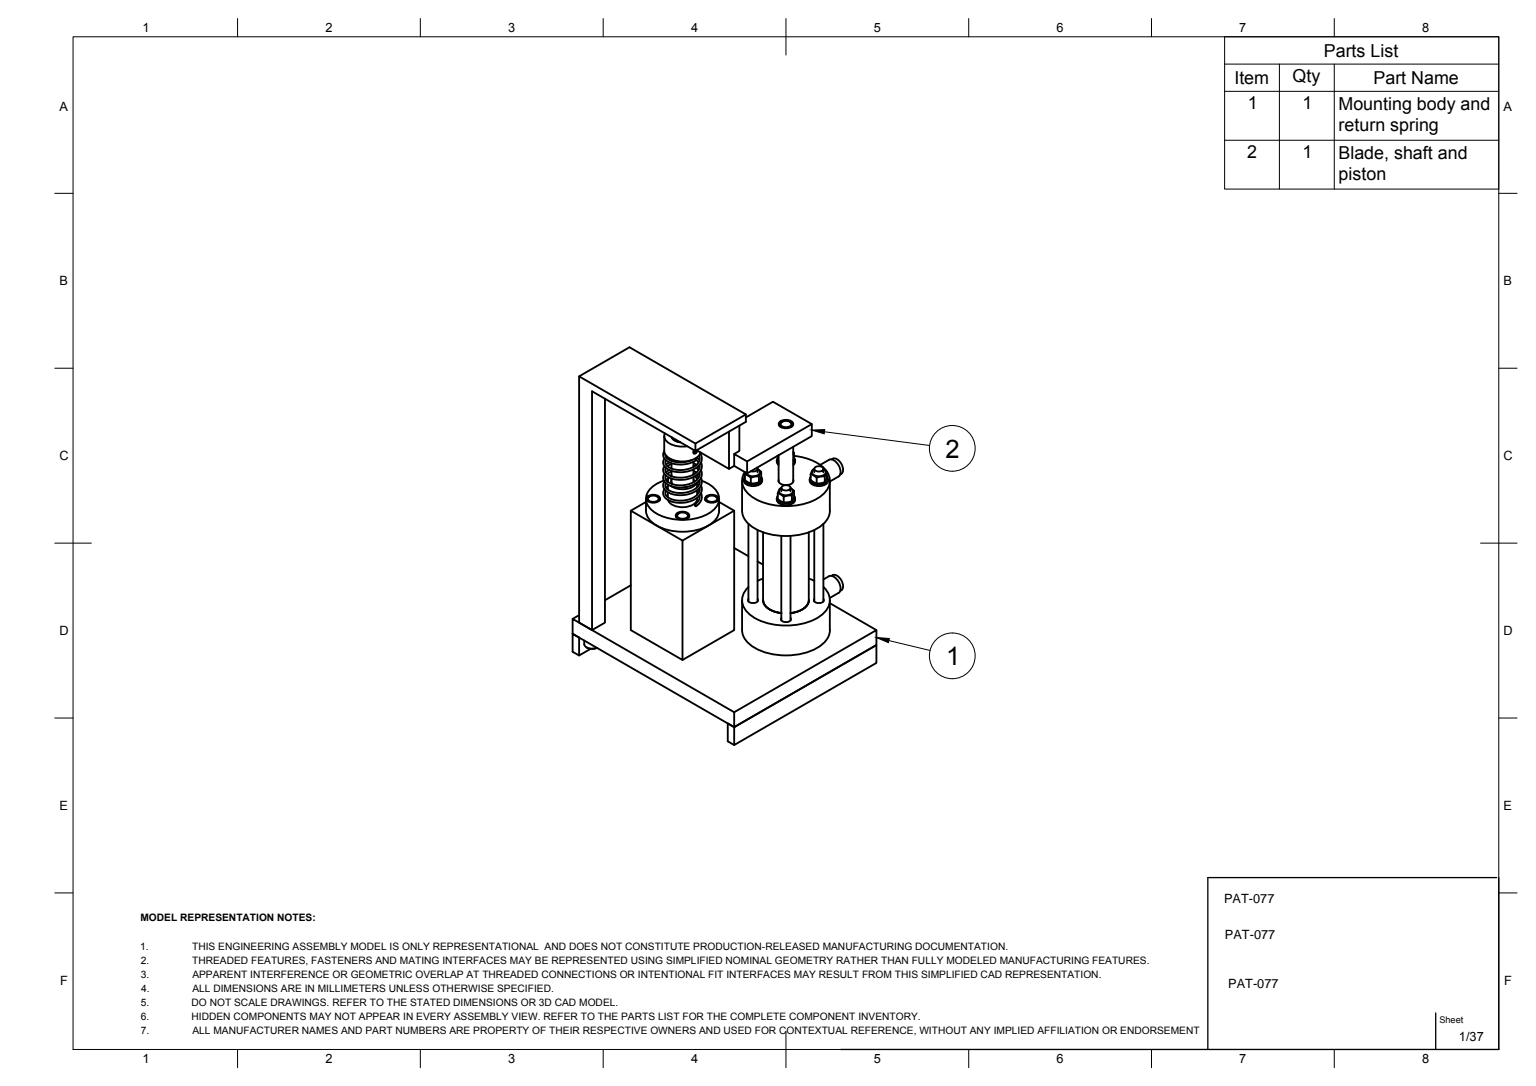
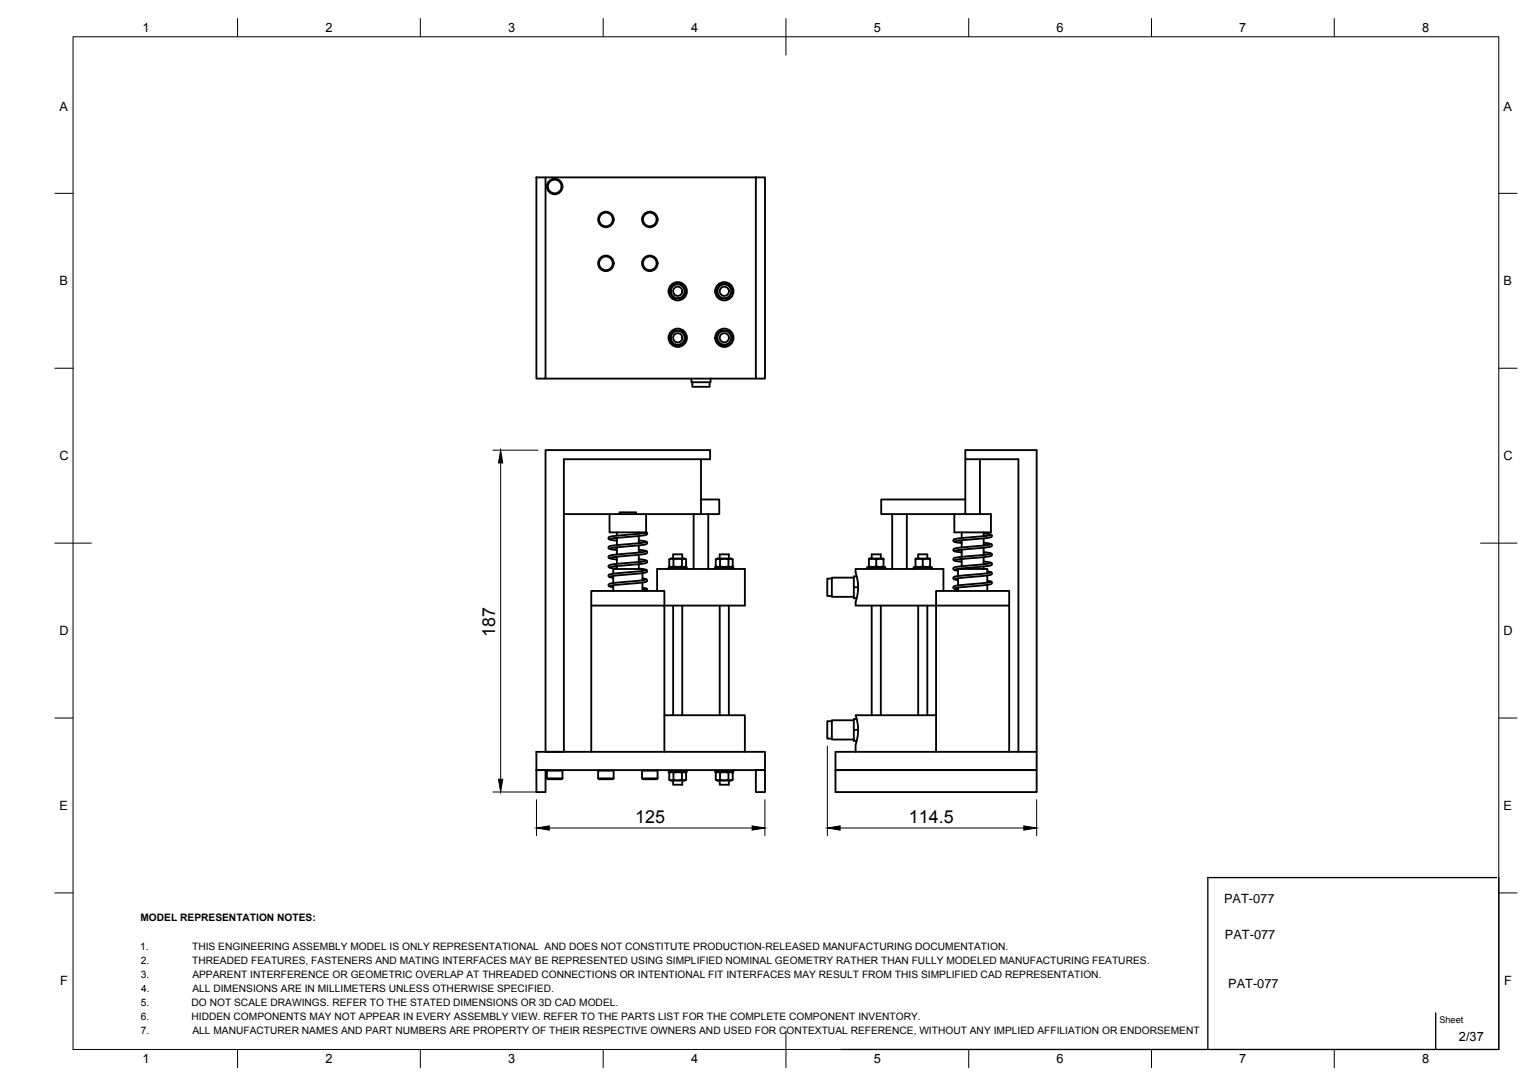
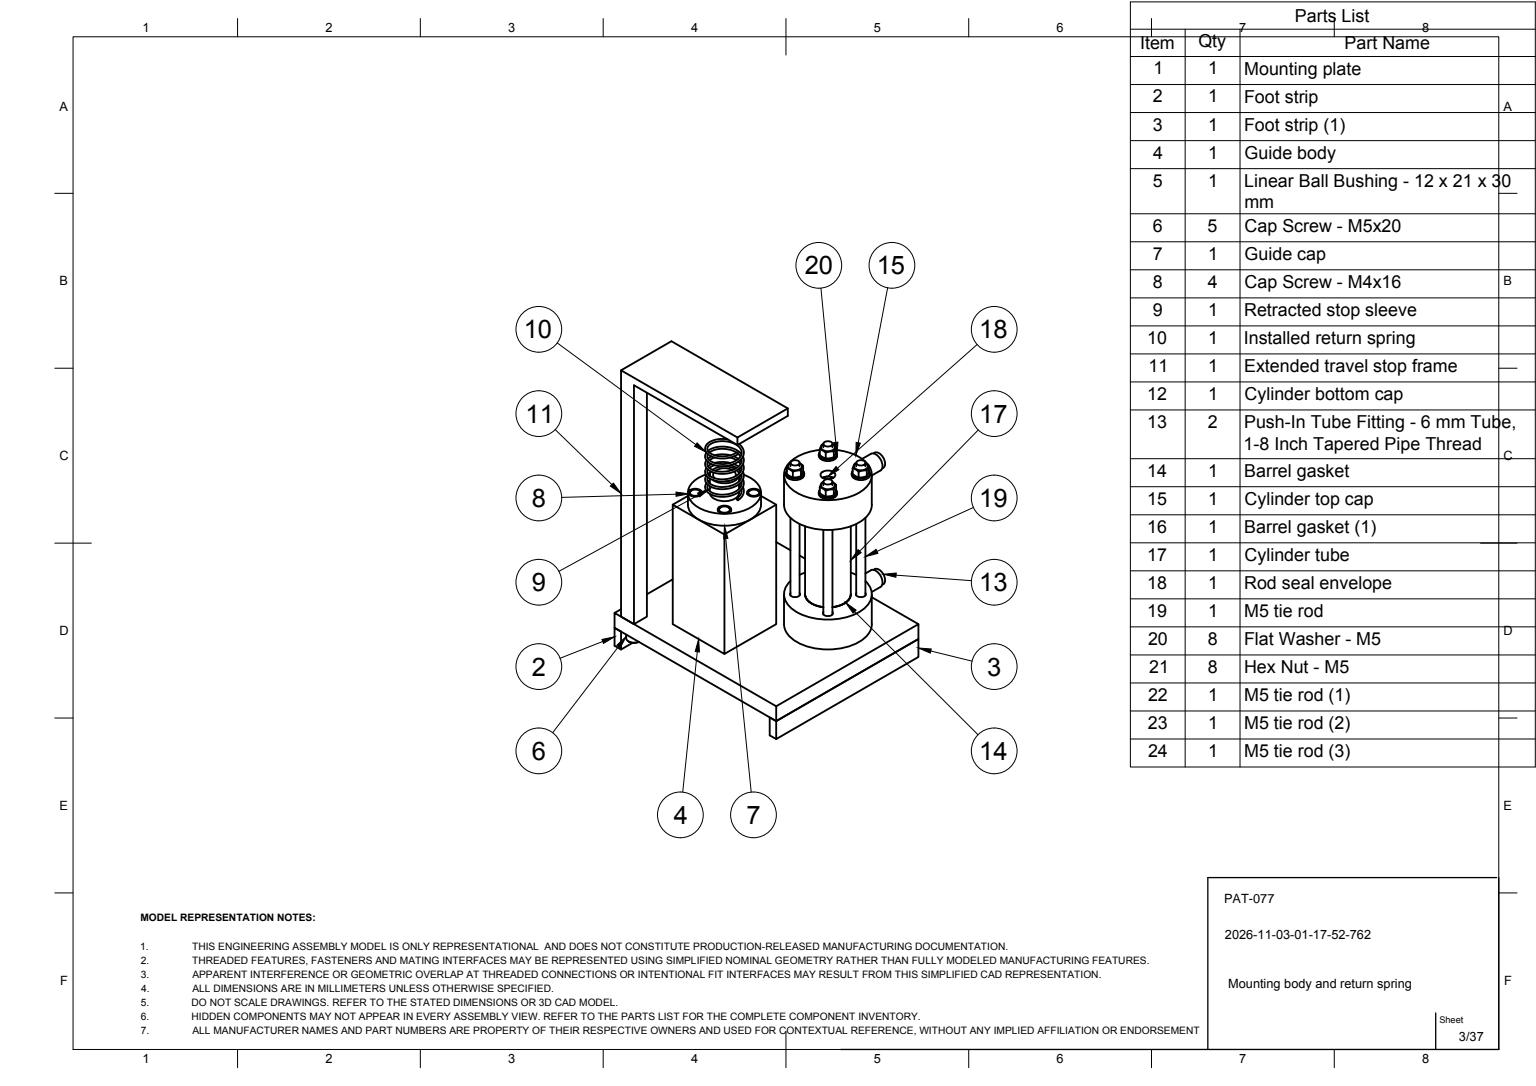
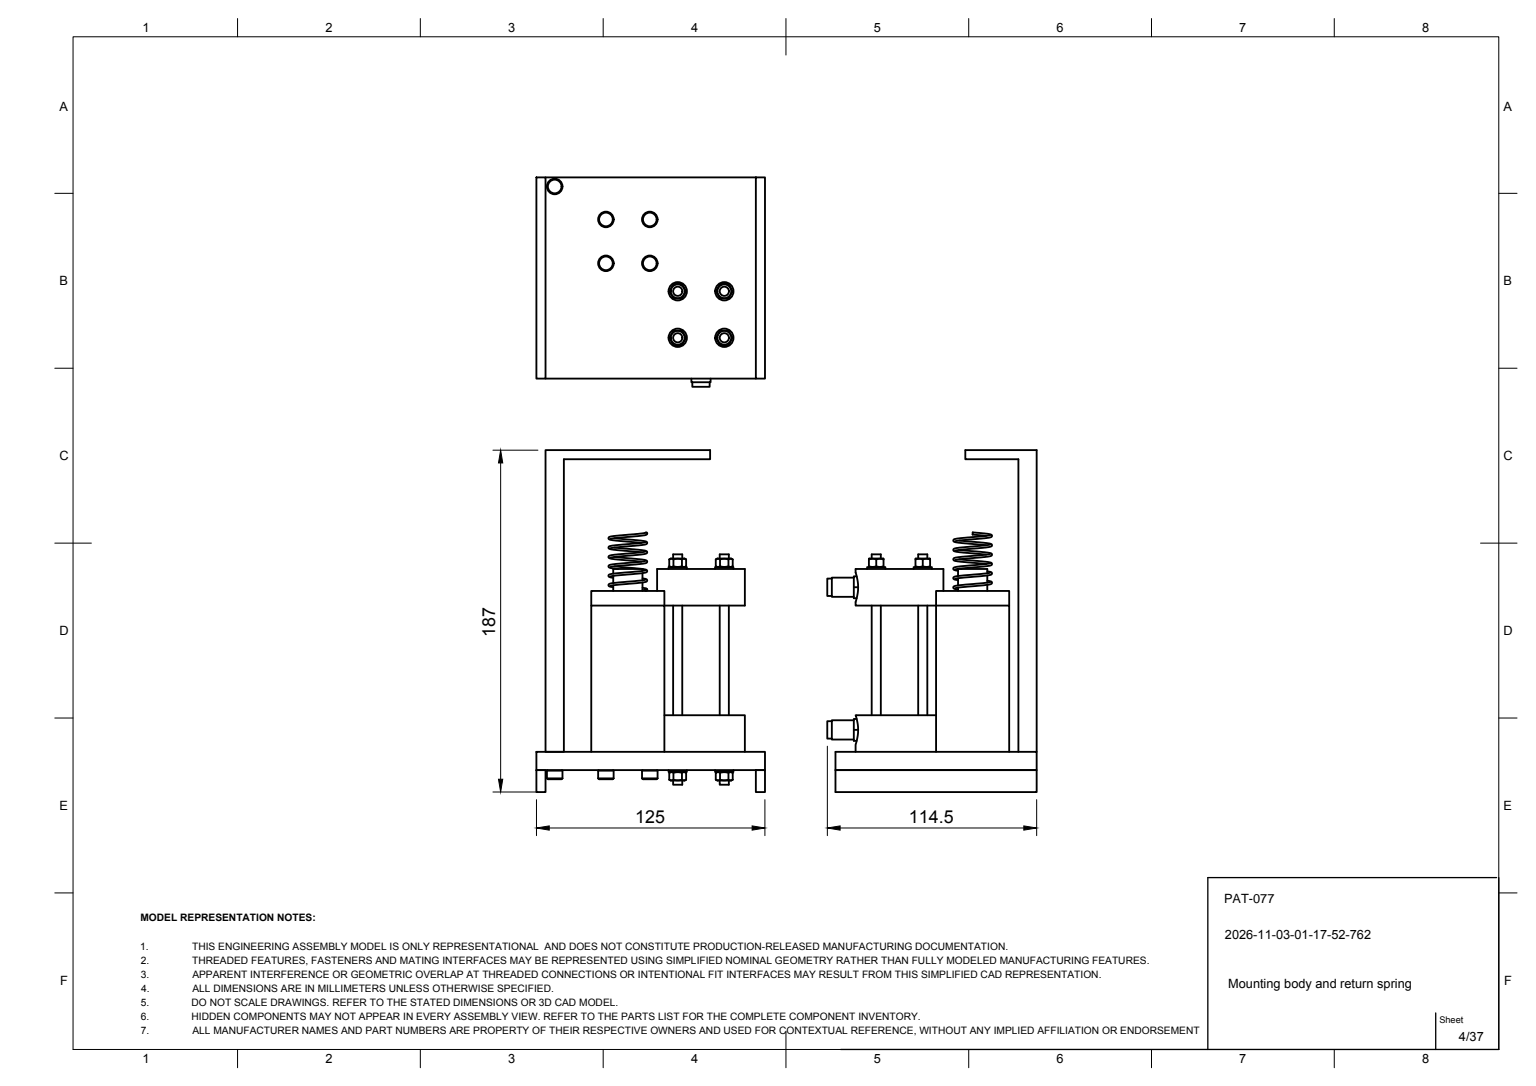
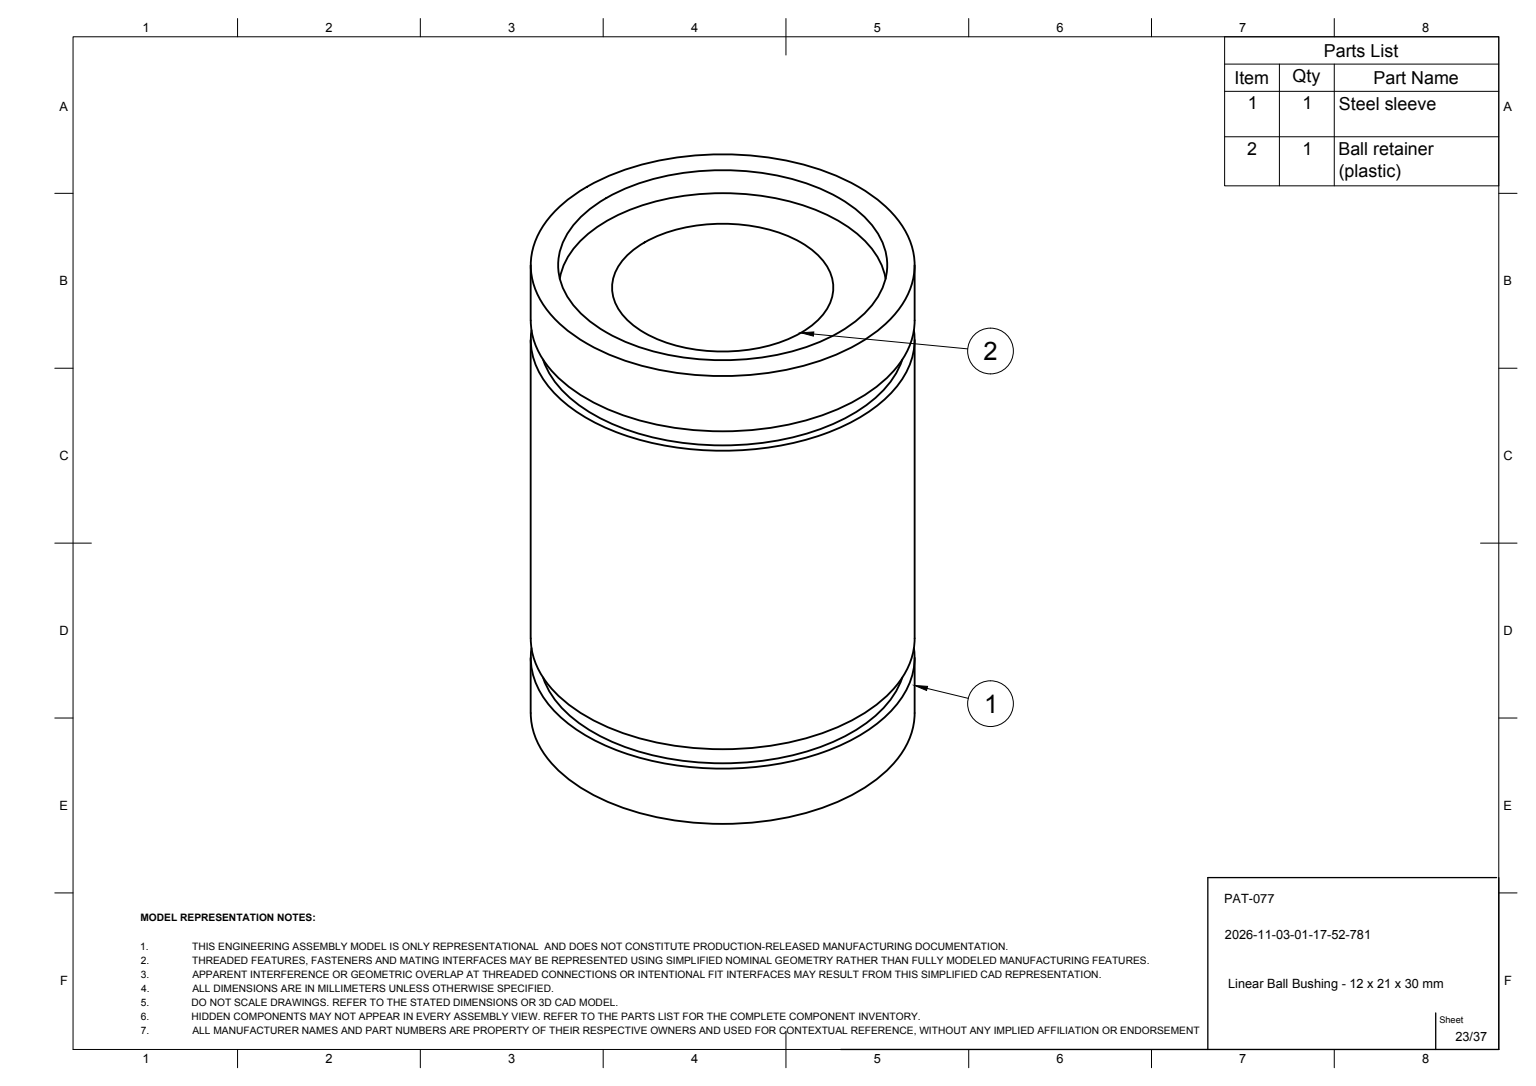
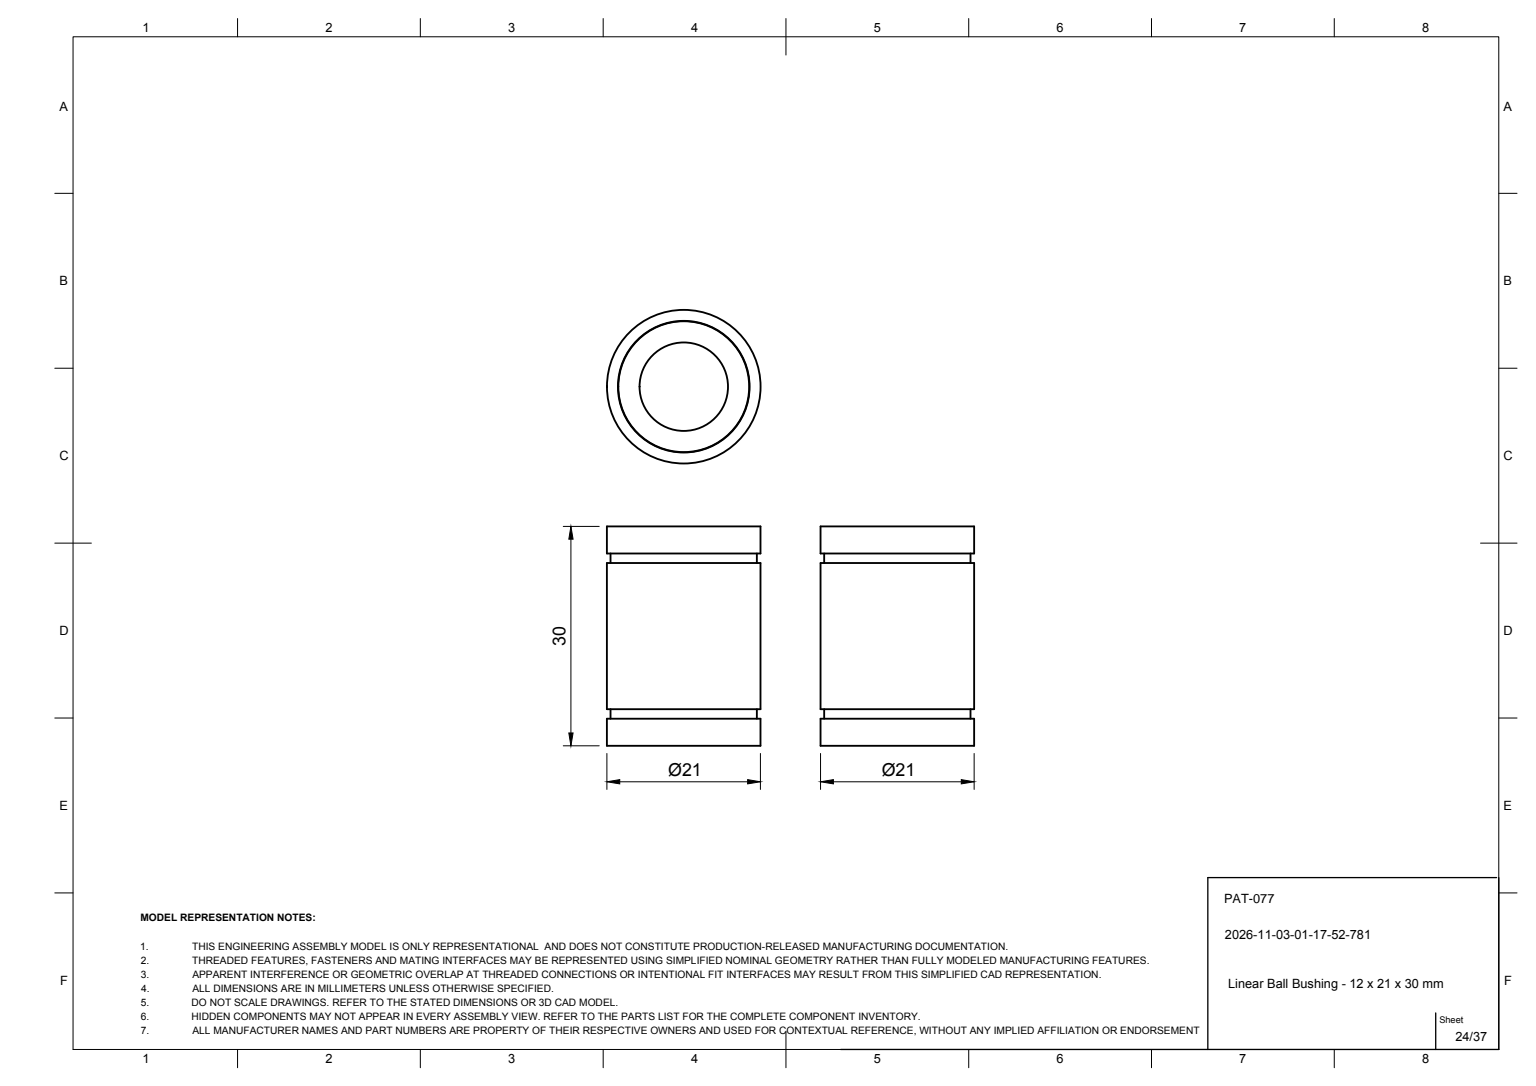
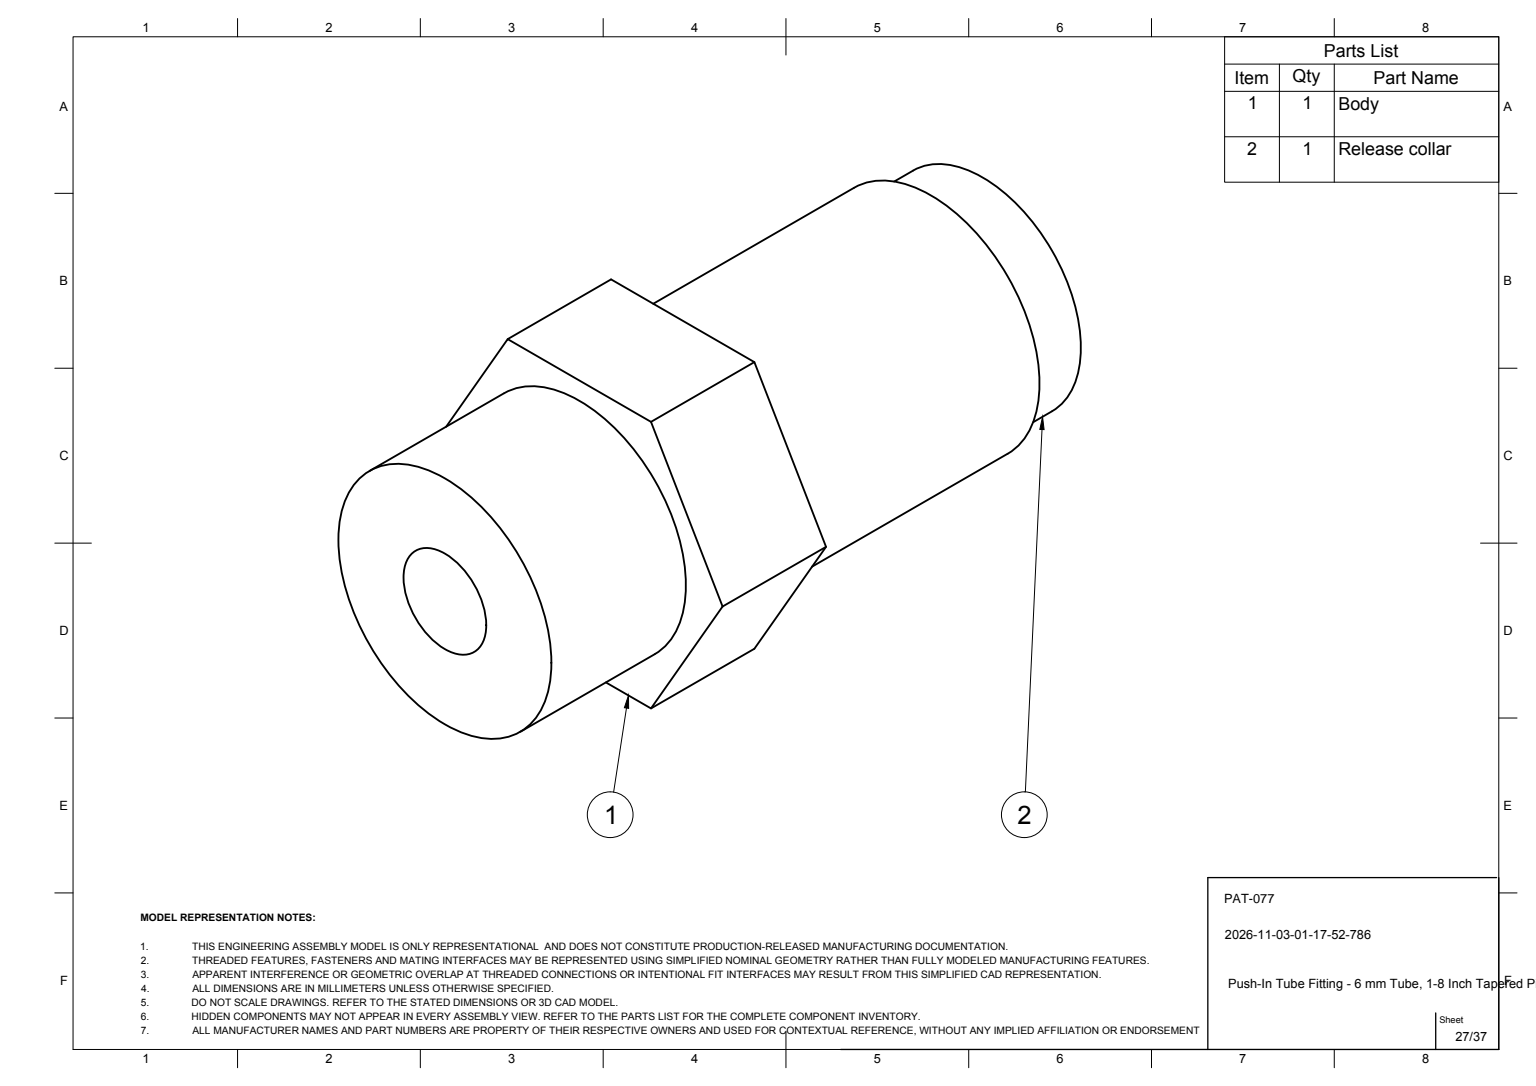
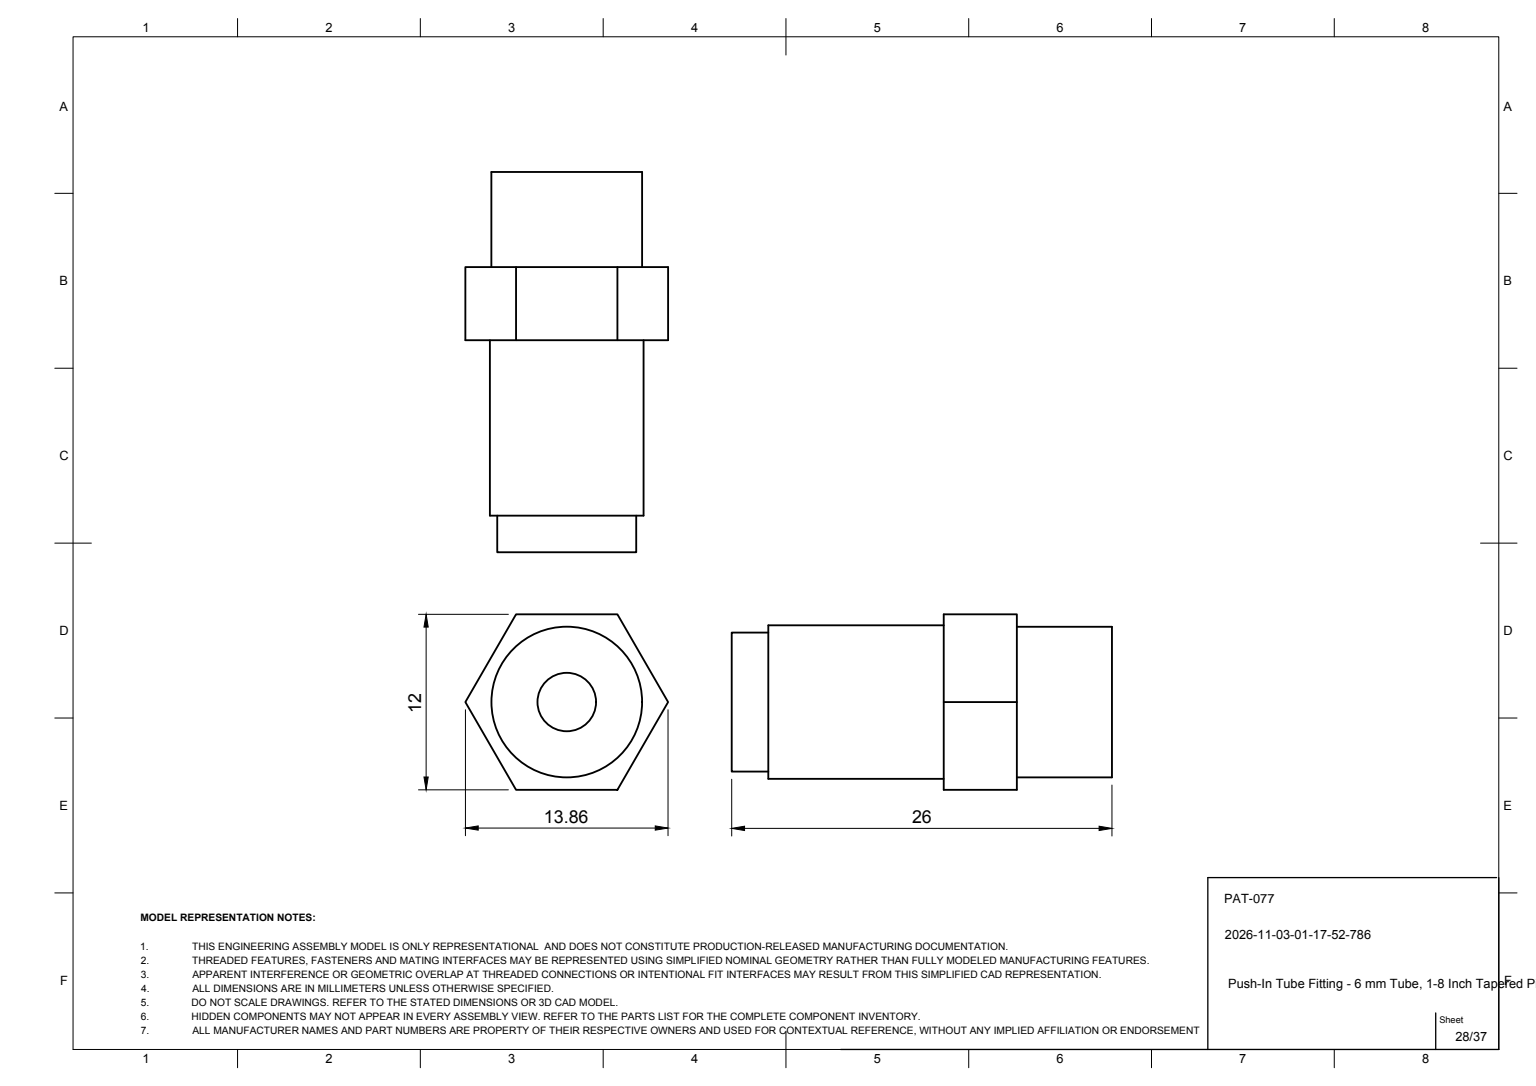
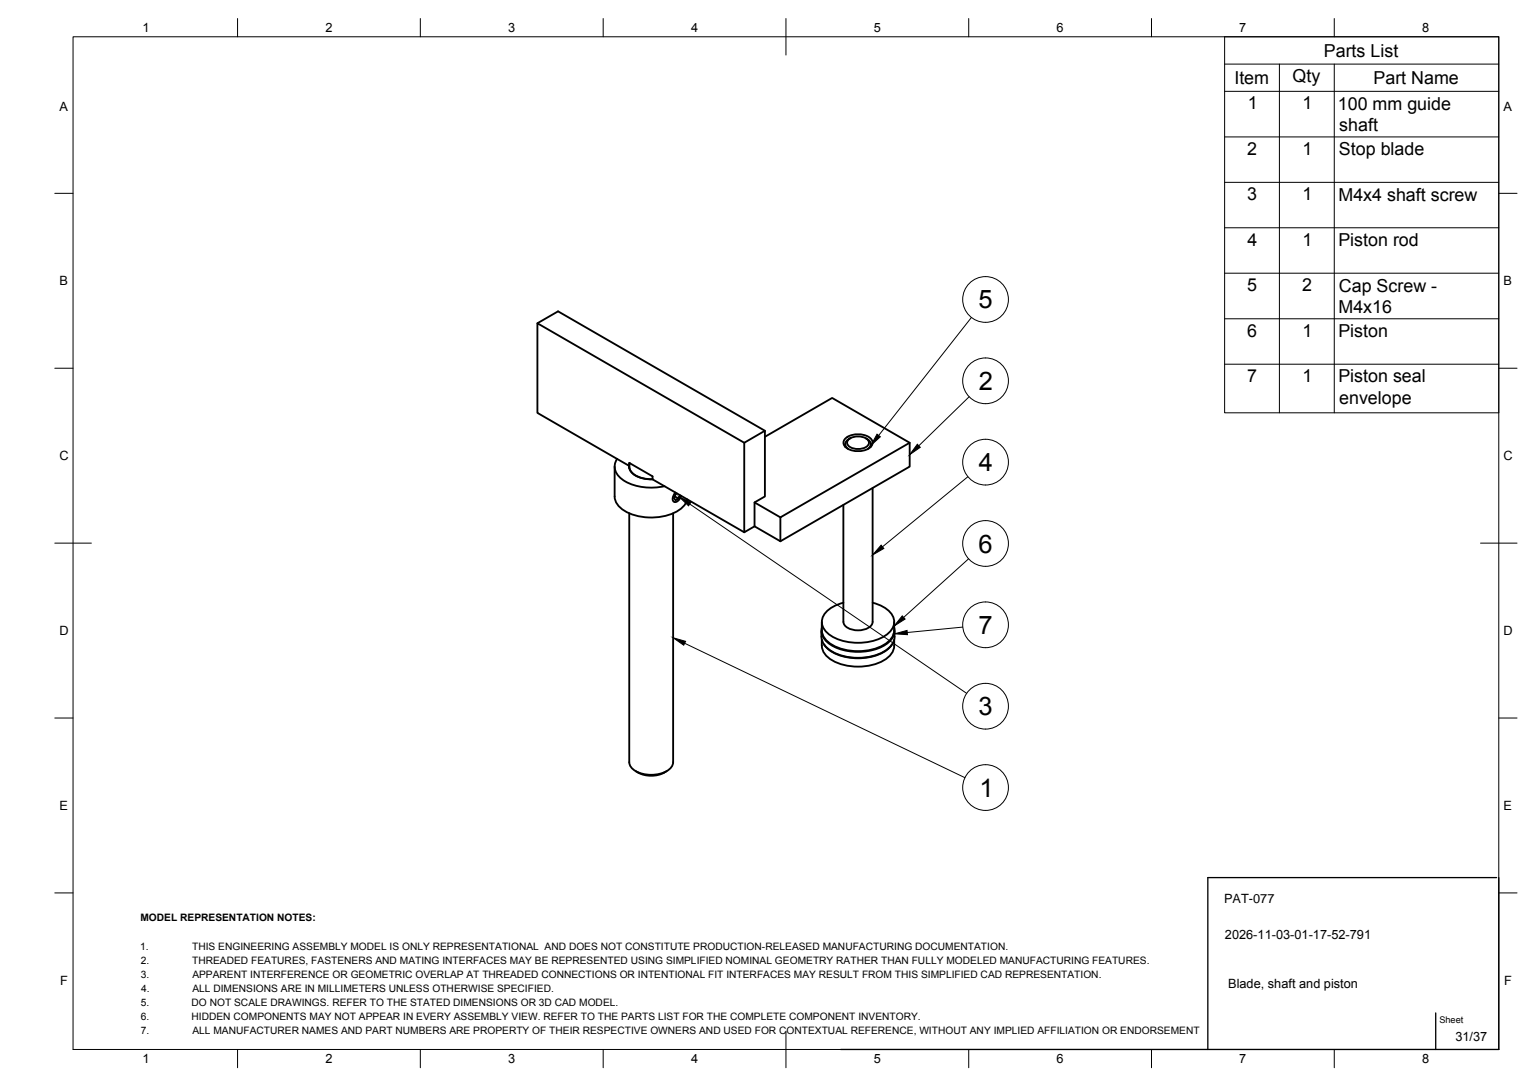
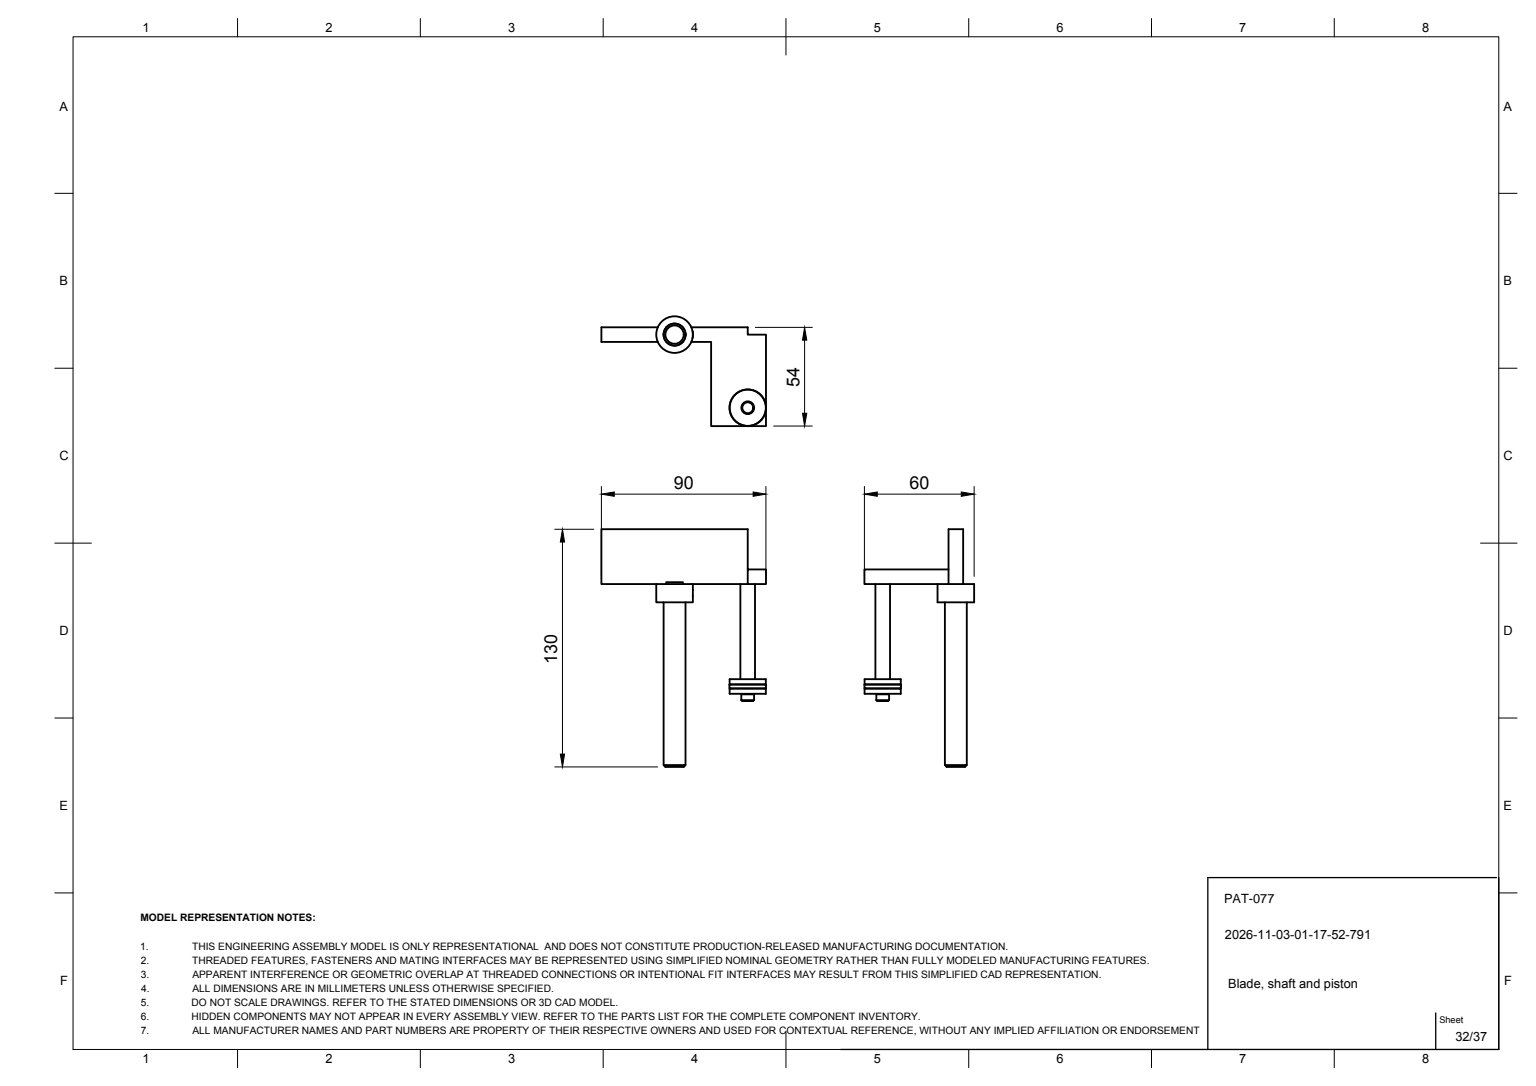
ISO-10303-21;
HEADER;
/* Generated by software containing ST-Developer
 * from STEP Tools, Inc. (www.steptools.com) 
 */

FILE_DESCRIPTION(
/* description */ ('Pallet stop with pneumatic fitting'),
/* implementation_level */ '2;1');

FILE_NAME(
/* name */ 'PAT-077',
/* time_stamp */ '2026-10-27T10:51:41-07:00',
/* author */ (''),
/* organization */ (''),
/* preprocessor_version */ 'ST-DEVELOPER v20.2',
/* originating_system */ 'Autodesk Translation Framework v15.17.0.0',
/* authorisation */ '');

FILE_SCHEMA (('AUTOMOTIVE_DESIGN { 1 0 10303 214 3 1 1 }'));
ENDSEC;

DATA;
#10=MECHANICAL_DESIGN_GEOMETRIC_PRESENTATION_REPRESENTATION('',(#357,#358,
#359,#360,#361,#362,#363,#364,#365,#366,#367,#368,#369,#370,#371,#372,#373,
#374,#375,#376,#377,#378,#379,#380,#381,#382,#383,#384,#385,#386,#387,#388),
#10265);
#11=(
BOUNDED_CURVE()
B_SPLINE_CURVE(2,(#9660,#9661,#9662),.UNSPECIFIED.,.F.,.F.)
B_SPLINE_CURVE_WITH_KNOTS((3,3),(0.140651836354967,0.670383167684795),
 .UNSPECIFIED.)
CURVE()
GEOMETRIC_REPRESENTATION_ITEM()
RATIONAL_B_SPLINE_CURVE((1.11602540378444,1.28867513459481,1.11602540378444))
REPRESENTATION_ITEM('')
);
#12=(
BOUNDED_CURVE()
B_SPLINE_CURVE(2,(#9664,#9665,#9666),.UNSPECIFIED.,.F.,.F.)
B_SPLINE_CURVE_WITH_KNOTS((3,3),(0.140651836354967,0.670383167684795),
 .UNSPECIFIED.)
CURVE()
GEOMETRIC_REPRESENTATION_ITEM()
RATIONAL_B_SPLINE_CURVE((1.11602540378444,1.28867513459481,1.11602540378444))
REPRESENTATION_ITEM('')
);
#13=(
BOUNDED_CURVE()
B_SPLINE_CURVE(2,(#9671,#9672,#9673),.UNSPECIFIED.,.F.,.F.)
B_SPLINE_CURVE_WITH_KNOTS((3,3),(0.140651836354967,0.670383167684795),
 .UNSPECIFIED.)
CURVE()
GEOMETRIC_REPRESENTATION_ITEM()
RATIONAL_B_SPLINE_CURVE((1.11602540378444,1.28867513459481,1.11602540378444))
REPRESENTATION_ITEM('')
);
#14=(
BOUNDED_CURVE()
B_SPLINE_CURVE(2,(#9675,#9676,#9677),.UNSPECIFIED.,.F.,.F.)
B_SPLINE_CURVE_WITH_KNOTS((3,3),(0.140651836354967,0.670383167684795),
 .UNSPECIFIED.)
CURVE()
GEOMETRIC_REPRESENTATION_ITEM()
RATIONAL_B_SPLINE_CURVE((1.11602540378444,1.28867513459481,1.11602540378444))
REPRESENTATION_ITEM('')
);
#15=(
BOUNDED_CURVE()
B_SPLINE_CURVE(2,(#9679,#9680,#9681),.UNSPECIFIED.,.F.,.F.)
B_SPLINE_CURVE_WITH_KNOTS((3,3),(0.140651836354967,0.670383167684795),
 .UNSPECIFIED.)
CURVE()
GEOMETRIC_REPRESENTATION_ITEM()
RATIONAL_B_SPLINE_CURVE((1.11602540378444,1.28867513459481,1.11602540378444))
REPRESENTATION_ITEM('')
);
#16=(
BOUNDED_CURVE()
B_SPLINE_CURVE(2,(#9682,#9683,#9684),.UNSPECIFIED.,.F.,.F.)
B_SPLINE_CURVE_WITH_KNOTS((3,3),(0.140651836354967,0.670383167684795),
 .UNSPECIFIED.)
CURVE()
GEOMETRIC_REPRESENTATION_ITEM()
RATIONAL_B_SPLINE_CURVE((1.11602540378444,1.28867513459481,1.11602540378444))
REPRESENTATION_ITEM('')
);
#17=(
BOUNDED_CURVE()
B_SPLINE_CURVE(2,(#9691,#9692,#9693),.UNSPECIFIED.,.F.,.F.)
B_SPLINE_CURVE_WITH_KNOTS((3,3),(0.140651836354967,0.670383167684795),
 .UNSPECIFIED.)
CURVE()
GEOMETRIC_REPRESENTATION_ITEM()
RATIONAL_B_SPLINE_CURVE((1.11602540378444,1.28867513459481,1.11602540378444))
REPRESENTATION_ITEM('')
);
#18=(
BOUNDED_CURVE()
B_SPLINE_CURVE(2,(#9695,#9696,#9697),.UNSPECIFIED.,.F.,.F.)
B_SPLINE_CURVE_WITH_KNOTS((3,3),(0.140651836354967,0.670383167684796),
 .UNSPECIFIED.)
CURVE()
GEOMETRIC_REPRESENTATION_ITEM()
RATIONAL_B_SPLINE_CURVE((1.11602540378444,1.28867513459481,1.11602540378444))
REPRESENTATION_ITEM('')
);
#19=(
BOUNDED_CURVE()
B_SPLINE_CURVE(2,(#9699,#9700,#9701),.UNSPECIFIED.,.F.,.F.)
B_SPLINE_CURVE_WITH_KNOTS((3,3),(0.140651836354967,0.670383167684795),
 .UNSPECIFIED.)
CURVE()
GEOMETRIC_REPRESENTATION_ITEM()
RATIONAL_B_SPLINE_CURVE((1.11602540378444,1.28867513459481,1.11602540378444))
REPRESENTATION_ITEM('')
);
#20=(
BOUNDED_CURVE()
B_SPLINE_CURVE(2,(#9703,#9704,#9705),.UNSPECIFIED.,.F.,.F.)
B_SPLINE_CURVE_WITH_KNOTS((3,3),(0.140651836354967,0.670383167684795),
 .UNSPECIFIED.)
CURVE()
GEOMETRIC_REPRESENTATION_ITEM()
RATIONAL_B_SPLINE_CURVE((1.11602540378444,1.28867513459482,1.11602540378444))
REPRESENTATION_ITEM('')
);
#21=(
BOUNDED_CURVE()
B_SPLINE_CURVE(2,(#9707,#9708,#9709),.UNSPECIFIED.,.F.,.F.)
B_SPLINE_CURVE_WITH_KNOTS((3,3),(0.140651836354967,0.670383167684795),
 .UNSPECIFIED.)
CURVE()
GEOMETRIC_REPRESENTATION_ITEM()
RATIONAL_B_SPLINE_CURVE((1.11602540378444,1.28867513459481,1.11602540378444))
REPRESENTATION_ITEM('')
);
#22=(
BOUNDED_CURVE()
B_SPLINE_CURVE(2,(#9710,#9711,#9712),.UNSPECIFIED.,.F.,.F.)
B_SPLINE_CURVE_WITH_KNOTS((3,3),(0.140651836354967,0.670383167684795),
 .UNSPECIFIED.)
CURVE()
GEOMETRIC_REPRESENTATION_ITEM()
RATIONAL_B_SPLINE_CURVE((1.11602540378444,1.28867513459481,1.11602540378444))
REPRESENTATION_ITEM('')
);
#23=ORIENTED_CLOSED_SHELL('',*,#5066,.F.);
#24=ORIENTED_CLOSED_SHELL('',*,#5078,.F.);
#25=CONICAL_SURFACE('',#5806,0.4,0.785398163397448);
#26=CONICAL_SURFACE('',#5810,0.41,0.785398163397448);
#27=CONICAL_SURFACE('',#5814,0.26,0.463647609000806);
#28=CONICAL_SURFACE('',#5818,0.225,0.785398163397448);
#29=CONICAL_SURFACE('',#5874,0.275,0.785398163397449);
#30=CONICAL_SURFACE('',#5885,0.47094010767585,1.0471975511966);
#31=CONICAL_SURFACE('',#5887,0.47094010767585,1.0471975511966);
#32=CONICAL_SURFACE('',#5987,0.55,0.785398163397448);
#33=CONICAL_SURFACE('',#6004,0.185,0.785398163397449);
#34=CONICAL_SURFACE('',#6010,0.325,0.785398163397448);
#35=CONICAL_SURFACE('',#6014,0.335,0.785398163397448);
#36=CONICAL_SURFACE('',#6018,0.21,0.463647609000806);
#37=CONICAL_SURFACE('',#6022,0.18,0.785398163397448);
#38=BREP_WITH_VOIDS('Body1',#5065,(#23));
#39=BREP_WITH_VOIDS('Body1',#5077,(#24));
#40=ITEM_DEFINED_TRANSFORMATION($,$,#5752,#5801);
#41=ITEM_DEFINED_TRANSFORMATION($,$,#5784,#5802);
#42=ITEM_DEFINED_TRANSFORMATION($,$,#5830,#5871);
#43=ITEM_DEFINED_TRANSFORMATION($,$,#5858,#5872);
#44=ITEM_DEFINED_TRANSFORMATION($,$,#5434,#6033);
#45=ITEM_DEFINED_TRANSFORMATION($,$,#5468,#6034);
#46=ITEM_DEFINED_TRANSFORMATION($,$,#5475,#6035);
#47=ITEM_DEFINED_TRANSFORMATION($,$,#5482,#6036);
#48=ITEM_DEFINED_TRANSFORMATION($,$,#5528,#6037);
#49=ITEM_DEFINED_TRANSFORMATION($,$,#5569,#6038);
#50=ITEM_DEFINED_TRANSFORMATION($,$,#5578,#6039);
#51=ITEM_DEFINED_TRANSFORMATION($,$,#5583,#6040);
#52=ITEM_DEFINED_TRANSFORMATION($,$,#5597,#6041);
#53=ITEM_DEFINED_TRANSFORMATION($,$,#5638,#6042);
#54=ITEM_DEFINED_TRANSFORMATION($,$,#5647,#6043);
#55=ITEM_DEFINED_TRANSFORMATION($,$,#5700,#6044);
#56=ITEM_DEFINED_TRANSFORMATION($,$,#5709,#6045);
#57=ITEM_DEFINED_TRANSFORMATION($,$,#5718,#6046);
#58=ITEM_DEFINED_TRANSFORMATION($,$,#5727,#6047);
#59=ITEM_DEFINED_TRANSFORMATION($,$,#5733,#6048);
#60=ITEM_DEFINED_TRANSFORMATION($,$,#5739,#6049);
#61=ITEM_DEFINED_TRANSFORMATION($,$,#5745,#6050);
#62=ITEM_DEFINED_TRANSFORMATION($,$,#5751,#6051);
#63=ITEM_DEFINED_TRANSFORMATION($,$,#5803,#6052);
#64=ITEM_DEFINED_TRANSFORMATION($,$,#5803,#6053);
#65=ITEM_DEFINED_TRANSFORMATION($,$,#5803,#6054);
#66=ITEM_DEFINED_TRANSFORMATION($,$,#5803,#6055);
#67=ITEM_DEFINED_TRANSFORMATION($,$,#6007,#6056);
#68=ITEM_DEFINED_TRANSFORMATION($,$,#6007,#6057);
#69=ITEM_DEFINED_TRANSFORMATION($,$,#6007,#6058);
#70=ITEM_DEFINED_TRANSFORMATION($,$,#6007,#6059);
#71=ITEM_DEFINED_TRANSFORMATION($,$,#5803,#6060);
#72=ITEM_DEFINED_TRANSFORMATION($,$,#5829,#6061);
#73=ITEM_DEFINED_TRANSFORMATION($,$,#5829,#6062);
#74=ITEM_DEFINED_TRANSFORMATION($,$,#5873,#6063);
#75=ITEM_DEFINED_TRANSFORMATION($,$,#5884,#6064);
#76=ITEM_DEFINED_TRANSFORMATION($,$,#5873,#6065);
#77=ITEM_DEFINED_TRANSFORMATION($,$,#5884,#6066);
#78=ITEM_DEFINED_TRANSFORMATION($,$,#5873,#6067);
#79=ITEM_DEFINED_TRANSFORMATION($,$,#5884,#6068);
#80=ITEM_DEFINED_TRANSFORMATION($,$,#5873,#6069);
#81=ITEM_DEFINED_TRANSFORMATION($,$,#5884,#6070);
#82=ITEM_DEFINED_TRANSFORMATION($,$,#5873,#6071);
#83=ITEM_DEFINED_TRANSFORMATION($,$,#5884,#6072);
#84=ITEM_DEFINED_TRANSFORMATION($,$,#5873,#6073);
#85=ITEM_DEFINED_TRANSFORMATION($,$,#5884,#6074);
#86=ITEM_DEFINED_TRANSFORMATION($,$,#5873,#6075);
#87=ITEM_DEFINED_TRANSFORMATION($,$,#5884,#6076);
#88=ITEM_DEFINED_TRANSFORMATION($,$,#5873,#6077);
#89=ITEM_DEFINED_TRANSFORMATION($,$,#5884,#6078);
#90=ITEM_DEFINED_TRANSFORMATION($,$,#5901,#6079);
#91=ITEM_DEFINED_TRANSFORMATION($,$,#5944,#6080);
#92=ITEM_DEFINED_TRANSFORMATION($,$,#5958,#6081);
#93=ITEM_DEFINED_TRANSFORMATION($,$,#5975,#6082);
#94=ITEM_DEFINED_TRANSFORMATION($,$,#5984,#6083);
#95=ITEM_DEFINED_TRANSFORMATION($,$,#5992,#6084);
#96=ITEM_DEFINED_TRANSFORMATION($,$,#6007,#6085);
#97=ITEM_DEFINED_TRANSFORMATION($,$,#6007,#6086);
#98=ITEM_DEFINED_TRANSFORMATION($,$,#5433,#6087);
#99=ITEM_DEFINED_TRANSFORMATION($,$,#5900,#6088);
#100=(
REPRESENTATION_RELATIONSHIP($,$,#10425,#10424)
REPRESENTATION_RELATIONSHIP_WITH_TRANSFORMATION(#40)
SHAPE_REPRESENTATION_RELATIONSHIP()
);
#101=(
REPRESENTATION_RELATIONSHIP($,$,#10426,#10424)
REPRESENTATION_RELATIONSHIP_WITH_TRANSFORMATION(#41)
SHAPE_REPRESENTATION_RELATIONSHIP()
);
#102=(
REPRESENTATION_RELATIONSHIP($,$,#10429,#10428)
REPRESENTATION_RELATIONSHIP_WITH_TRANSFORMATION(#42)
SHAPE_REPRESENTATION_RELATIONSHIP()
);
#103=(
REPRESENTATION_RELATIONSHIP($,$,#10430,#10428)
REPRESENTATION_RELATIONSHIP_WITH_TRANSFORMATION(#43)
SHAPE_REPRESENTATION_RELATIONSHIP()
);
#104=(
REPRESENTATION_RELATIONSHIP($,$,#10406,#10405)
REPRESENTATION_RELATIONSHIP_WITH_TRANSFORMATION(#44)
SHAPE_REPRESENTATION_RELATIONSHIP()
);
#105=(
REPRESENTATION_RELATIONSHIP($,$,#10407,#10405)
REPRESENTATION_RELATIONSHIP_WITH_TRANSFORMATION(#45)
SHAPE_REPRESENTATION_RELATIONSHIP()
);
#106=(
REPRESENTATION_RELATIONSHIP($,$,#10408,#10405)
REPRESENTATION_RELATIONSHIP_WITH_TRANSFORMATION(#46)
SHAPE_REPRESENTATION_RELATIONSHIP()
);
#107=(
REPRESENTATION_RELATIONSHIP($,$,#10409,#10405)
REPRESENTATION_RELATIONSHIP_WITH_TRANSFORMATION(#47)
SHAPE_REPRESENTATION_RELATIONSHIP()
);
#108=(
REPRESENTATION_RELATIONSHIP($,$,#10410,#10405)
REPRESENTATION_RELATIONSHIP_WITH_TRANSFORMATION(#48)
SHAPE_REPRESENTATION_RELATIONSHIP()
);
#109=(
REPRESENTATION_RELATIONSHIP($,$,#10411,#10405)
REPRESENTATION_RELATIONSHIP_WITH_TRANSFORMATION(#49)
SHAPE_REPRESENTATION_RELATIONSHIP()
);
#110=(
REPRESENTATION_RELATIONSHIP($,$,#10412,#10405)
REPRESENTATION_RELATIONSHIP_WITH_TRANSFORMATION(#50)
SHAPE_REPRESENTATION_RELATIONSHIP()
);
#111=(
REPRESENTATION_RELATIONSHIP($,$,#10413,#10405)
REPRESENTATION_RELATIONSHIP_WITH_TRANSFORMATION(#51)
SHAPE_REPRESENTATION_RELATIONSHIP()
);
#112=(
REPRESENTATION_RELATIONSHIP($,$,#10414,#10405)
REPRESENTATION_RELATIONSHIP_WITH_TRANSFORMATION(#52)
SHAPE_REPRESENTATION_RELATIONSHIP()
);
#113=(
REPRESENTATION_RELATIONSHIP($,$,#10415,#10405)
REPRESENTATION_RELATIONSHIP_WITH_TRANSFORMATION(#53)
SHAPE_REPRESENTATION_RELATIONSHIP()
);
#114=(
REPRESENTATION_RELATIONSHIP($,$,#10416,#10405)
REPRESENTATION_RELATIONSHIP_WITH_TRANSFORMATION(#54)
SHAPE_REPRESENTATION_RELATIONSHIP()
);
#115=(
REPRESENTATION_RELATIONSHIP($,$,#10417,#10405)
REPRESENTATION_RELATIONSHIP_WITH_TRANSFORMATION(#55)
SHAPE_REPRESENTATION_RELATIONSHIP()
);
#116=(
REPRESENTATION_RELATIONSHIP($,$,#10418,#10405)
REPRESENTATION_RELATIONSHIP_WITH_TRANSFORMATION(#56)
SHAPE_REPRESENTATION_RELATIONSHIP()
);
#117=(
REPRESENTATION_RELATIONSHIP($,$,#10419,#10405)
REPRESENTATION_RELATIONSHIP_WITH_TRANSFORMATION(#57)
SHAPE_REPRESENTATION_RELATIONSHIP()
);
#118=(
REPRESENTATION_RELATIONSHIP($,$,#10420,#10405)
REPRESENTATION_RELATIONSHIP_WITH_TRANSFORMATION(#58)
SHAPE_REPRESENTATION_RELATIONSHIP()
);
#119=(
REPRESENTATION_RELATIONSHIP($,$,#10421,#10405)
REPRESENTATION_RELATIONSHIP_WITH_TRANSFORMATION(#59)
SHAPE_REPRESENTATION_RELATIONSHIP()
);
#120=(
REPRESENTATION_RELATIONSHIP($,$,#10422,#10405)
REPRESENTATION_RELATIONSHIP_WITH_TRANSFORMATION(#60)
SHAPE_REPRESENTATION_RELATIONSHIP()
);
#121=(
REPRESENTATION_RELATIONSHIP($,$,#10423,#10405)
REPRESENTATION_RELATIONSHIP_WITH_TRANSFORMATION(#61)
SHAPE_REPRESENTATION_RELATIONSHIP()
);
#122=(
REPRESENTATION_RELATIONSHIP($,$,#10424,#10405)
REPRESENTATION_RELATIONSHIP_WITH_TRANSFORMATION(#62)
SHAPE_REPRESENTATION_RELATIONSHIP()
);
#123=(
REPRESENTATION_RELATIONSHIP($,$,#10427,#10405)
REPRESENTATION_RELATIONSHIP_WITH_TRANSFORMATION(#63)
SHAPE_REPRESENTATION_RELATIONSHIP()
);
#124=(
REPRESENTATION_RELATIONSHIP($,$,#10427,#10405)
REPRESENTATION_RELATIONSHIP_WITH_TRANSFORMATION(#64)
SHAPE_REPRESENTATION_RELATIONSHIP()
);
#125=(
REPRESENTATION_RELATIONSHIP($,$,#10427,#10405)
REPRESENTATION_RELATIONSHIP_WITH_TRANSFORMATION(#65)
SHAPE_REPRESENTATION_RELATIONSHIP()
);
#126=(
REPRESENTATION_RELATIONSHIP($,$,#10427,#10405)
REPRESENTATION_RELATIONSHIP_WITH_TRANSFORMATION(#66)
SHAPE_REPRESENTATION_RELATIONSHIP()
);
#127=(
REPRESENTATION_RELATIONSHIP($,$,#10440,#10405)
REPRESENTATION_RELATIONSHIP_WITH_TRANSFORMATION(#67)
SHAPE_REPRESENTATION_RELATIONSHIP()
);
#128=(
REPRESENTATION_RELATIONSHIP($,$,#10440,#10405)
REPRESENTATION_RELATIONSHIP_WITH_TRANSFORMATION(#68)
SHAPE_REPRESENTATION_RELATIONSHIP()
);
#129=(
REPRESENTATION_RELATIONSHIP($,$,#10440,#10405)
REPRESENTATION_RELATIONSHIP_WITH_TRANSFORMATION(#69)
SHAPE_REPRESENTATION_RELATIONSHIP()
);
#130=(
REPRESENTATION_RELATIONSHIP($,$,#10440,#10405)
REPRESENTATION_RELATIONSHIP_WITH_TRANSFORMATION(#70)
SHAPE_REPRESENTATION_RELATIONSHIP()
);
#131=(
REPRESENTATION_RELATIONSHIP($,$,#10427,#10405)
REPRESENTATION_RELATIONSHIP_WITH_TRANSFORMATION(#71)
SHAPE_REPRESENTATION_RELATIONSHIP()
);
#132=(
REPRESENTATION_RELATIONSHIP($,$,#10428,#10405)
REPRESENTATION_RELATIONSHIP_WITH_TRANSFORMATION(#72)
SHAPE_REPRESENTATION_RELATIONSHIP()
);
#133=(
REPRESENTATION_RELATIONSHIP($,$,#10428,#10405)
REPRESENTATION_RELATIONSHIP_WITH_TRANSFORMATION(#73)
SHAPE_REPRESENTATION_RELATIONSHIP()
);
#134=(
REPRESENTATION_RELATIONSHIP($,$,#10431,#10405)
REPRESENTATION_RELATIONSHIP_WITH_TRANSFORMATION(#74)
SHAPE_REPRESENTATION_RELATIONSHIP()
);
#135=(
REPRESENTATION_RELATIONSHIP($,$,#10432,#10405)
REPRESENTATION_RELATIONSHIP_WITH_TRANSFORMATION(#75)
SHAPE_REPRESENTATION_RELATIONSHIP()
);
#136=(
REPRESENTATION_RELATIONSHIP($,$,#10431,#10405)
REPRESENTATION_RELATIONSHIP_WITH_TRANSFORMATION(#76)
SHAPE_REPRESENTATION_RELATIONSHIP()
);
#137=(
REPRESENTATION_RELATIONSHIP($,$,#10432,#10405)
REPRESENTATION_RELATIONSHIP_WITH_TRANSFORMATION(#77)
SHAPE_REPRESENTATION_RELATIONSHIP()
);
#138=(
REPRESENTATION_RELATIONSHIP($,$,#10431,#10405)
REPRESENTATION_RELATIONSHIP_WITH_TRANSFORMATION(#78)
SHAPE_REPRESENTATION_RELATIONSHIP()
);
#139=(
REPRESENTATION_RELATIONSHIP($,$,#10432,#10405)
REPRESENTATION_RELATIONSHIP_WITH_TRANSFORMATION(#79)
SHAPE_REPRESENTATION_RELATIONSHIP()
);
#140=(
REPRESENTATION_RELATIONSHIP($,$,#10431,#10405)
REPRESENTATION_RELATIONSHIP_WITH_TRANSFORMATION(#80)
SHAPE_REPRESENTATION_RELATIONSHIP()
);
#141=(
REPRESENTATION_RELATIONSHIP($,$,#10432,#10405)
REPRESENTATION_RELATIONSHIP_WITH_TRANSFORMATION(#81)
SHAPE_REPRESENTATION_RELATIONSHIP()
);
#142=(
REPRESENTATION_RELATIONSHIP($,$,#10431,#10405)
REPRESENTATION_RELATIONSHIP_WITH_TRANSFORMATION(#82)
SHAPE_REPRESENTATION_RELATIONSHIP()
);
#143=(
REPRESENTATION_RELATIONSHIP($,$,#10432,#10405)
REPRESENTATION_RELATIONSHIP_WITH_TRANSFORMATION(#83)
SHAPE_REPRESENTATION_RELATIONSHIP()
);
#144=(
REPRESENTATION_RELATIONSHIP($,$,#10431,#10405)
REPRESENTATION_RELATIONSHIP_WITH_TRANSFORMATION(#84)
SHAPE_REPRESENTATION_RELATIONSHIP()
);
#145=(
REPRESENTATION_RELATIONSHIP($,$,#10432,#10405)
REPRESENTATION_RELATIONSHIP_WITH_TRANSFORMATION(#85)
SHAPE_REPRESENTATION_RELATIONSHIP()
);
#146=(
REPRESENTATION_RELATIONSHIP($,$,#10431,#10405)
REPRESENTATION_RELATIONSHIP_WITH_TRANSFORMATION(#86)
SHAPE_REPRESENTATION_RELATIONSHIP()
);
#147=(
REPRESENTATION_RELATIONSHIP($,$,#10432,#10405)
REPRESENTATION_RELATIONSHIP_WITH_TRANSFORMATION(#87)
SHAPE_REPRESENTATION_RELATIONSHIP()
);
#148=(
REPRESENTATION_RELATIONSHIP($,$,#10431,#10405)
REPRESENTATION_RELATIONSHIP_WITH_TRANSFORMATION(#88)
SHAPE_REPRESENTATION_RELATIONSHIP()
);
#149=(
REPRESENTATION_RELATIONSHIP($,$,#10432,#10405)
REPRESENTATION_RELATIONSHIP_WITH_TRANSFORMATION(#89)
SHAPE_REPRESENTATION_RELATIONSHIP()
);
#150=(
REPRESENTATION_RELATIONSHIP($,$,#10434,#10433)
REPRESENTATION_RELATIONSHIP_WITH_TRANSFORMATION(#90)
SHAPE_REPRESENTATION_RELATIONSHIP()
);
#151=(
REPRESENTATION_RELATIONSHIP($,$,#10435,#10433)
REPRESENTATION_RELATIONSHIP_WITH_TRANSFORMATION(#91)
SHAPE_REPRESENTATION_RELATIONSHIP()
);
#152=(
REPRESENTATION_RELATIONSHIP($,$,#10436,#10433)
REPRESENTATION_RELATIONSHIP_WITH_TRANSFORMATION(#92)
SHAPE_REPRESENTATION_RELATIONSHIP()
);
#153=(
REPRESENTATION_RELATIONSHIP($,$,#10437,#10433)
REPRESENTATION_RELATIONSHIP_WITH_TRANSFORMATION(#93)
SHAPE_REPRESENTATION_RELATIONSHIP()
);
#154=(
REPRESENTATION_RELATIONSHIP($,$,#10438,#10433)
REPRESENTATION_RELATIONSHIP_WITH_TRANSFORMATION(#94)
SHAPE_REPRESENTATION_RELATIONSHIP()
);
#155=(
REPRESENTATION_RELATIONSHIP($,$,#10439,#10433)
REPRESENTATION_RELATIONSHIP_WITH_TRANSFORMATION(#95)
SHAPE_REPRESENTATION_RELATIONSHIP()
);
#156=(
REPRESENTATION_RELATIONSHIP($,$,#10440,#10433)
REPRESENTATION_RELATIONSHIP_WITH_TRANSFORMATION(#96)
SHAPE_REPRESENTATION_RELATIONSHIP()
);
#157=(
REPRESENTATION_RELATIONSHIP($,$,#10440,#10433)
REPRESENTATION_RELATIONSHIP_WITH_TRANSFORMATION(#97)
SHAPE_REPRESENTATION_RELATIONSHIP()
);
#158=(
REPRESENTATION_RELATIONSHIP($,$,#10405,#10404)
REPRESENTATION_RELATIONSHIP_WITH_TRANSFORMATION(#98)
SHAPE_REPRESENTATION_RELATIONSHIP()
);
#159=(
REPRESENTATION_RELATIONSHIP($,$,#10433,#10404)
REPRESENTATION_RELATIONSHIP_WITH_TRANSFORMATION(#99)
SHAPE_REPRESENTATION_RELATIONSHIP()
);
#160=CONTEXT_DEPENDENT_SHAPE_REPRESENTATION(#100,#10330);
#161=CONTEXT_DEPENDENT_SHAPE_REPRESENTATION(#101,#10331);
#162=CONTEXT_DEPENDENT_SHAPE_REPRESENTATION(#102,#10336);
#163=CONTEXT_DEPENDENT_SHAPE_REPRESENTATION(#103,#10337);
#164=CONTEXT_DEPENDENT_SHAPE_REPRESENTATION(#104,#10348);
#165=CONTEXT_DEPENDENT_SHAPE_REPRESENTATION(#105,#10349);
#166=CONTEXT_DEPENDENT_SHAPE_REPRESENTATION(#106,#10350);
#167=CONTEXT_DEPENDENT_SHAPE_REPRESENTATION(#107,#10351);
#168=CONTEXT_DEPENDENT_SHAPE_REPRESENTATION(#108,#10352);
#169=CONTEXT_DEPENDENT_SHAPE_REPRESENTATION(#109,#10353);
#170=CONTEXT_DEPENDENT_SHAPE_REPRESENTATION(#110,#10354);
#171=CONTEXT_DEPENDENT_SHAPE_REPRESENTATION(#111,#10355);
#172=CONTEXT_DEPENDENT_SHAPE_REPRESENTATION(#112,#10356);
#173=CONTEXT_DEPENDENT_SHAPE_REPRESENTATION(#113,#10357);
#174=CONTEXT_DEPENDENT_SHAPE_REPRESENTATION(#114,#10358);
#175=CONTEXT_DEPENDENT_SHAPE_REPRESENTATION(#115,#10359);
#176=CONTEXT_DEPENDENT_SHAPE_REPRESENTATION(#116,#10360);
#177=CONTEXT_DEPENDENT_SHAPE_REPRESENTATION(#117,#10361);
#178=CONTEXT_DEPENDENT_SHAPE_REPRESENTATION(#118,#10362);
#179=CONTEXT_DEPENDENT_SHAPE_REPRESENTATION(#119,#10363);
#180=CONTEXT_DEPENDENT_SHAPE_REPRESENTATION(#120,#10364);
#181=CONTEXT_DEPENDENT_SHAPE_REPRESENTATION(#121,#10365);
#182=CONTEXT_DEPENDENT_SHAPE_REPRESENTATION(#122,#10366);
#183=CONTEXT_DEPENDENT_SHAPE_REPRESENTATION(#123,#10367);
#184=CONTEXT_DEPENDENT_SHAPE_REPRESENTATION(#124,#10368);
#185=CONTEXT_DEPENDENT_SHAPE_REPRESENTATION(#125,#10369);
#186=CONTEXT_DEPENDENT_SHAPE_REPRESENTATION(#126,#10370);
#187=CONTEXT_DEPENDENT_SHAPE_REPRESENTATION(#127,#10371);
#188=CONTEXT_DEPENDENT_SHAPE_REPRESENTATION(#128,#10372);
#189=CONTEXT_DEPENDENT_SHAPE_REPRESENTATION(#129,#10373);
#190=CONTEXT_DEPENDENT_SHAPE_REPRESENTATION(#130,#10374);
#191=CONTEXT_DEPENDENT_SHAPE_REPRESENTATION(#131,#10375);
#192=CONTEXT_DEPENDENT_SHAPE_REPRESENTATION(#132,#10376);
#193=CONTEXT_DEPENDENT_SHAPE_REPRESENTATION(#133,#10377);
#194=CONTEXT_DEPENDENT_SHAPE_REPRESENTATION(#134,#10378);
#195=CONTEXT_DEPENDENT_SHAPE_REPRESENTATION(#135,#10379);
#196=CONTEXT_DEPENDENT_SHAPE_REPRESENTATION(#136,#10380);
#197=CONTEXT_DEPENDENT_SHAPE_REPRESENTATION(#137,#10381);
#198=CONTEXT_DEPENDENT_SHAPE_REPRESENTATION(#138,#10382);
#199=CONTEXT_DEPENDENT_SHAPE_REPRESENTATION(#139,#10383);
#200=CONTEXT_DEPENDENT_SHAPE_REPRESENTATION(#140,#10384);
#201=CONTEXT_DEPENDENT_SHAPE_REPRESENTATION(#141,#10385);
#202=CONTEXT_DEPENDENT_SHAPE_REPRESENTATION(#142,#10386);
#203=CONTEXT_DEPENDENT_SHAPE_REPRESENTATION(#143,#10387);
#204=CONTEXT_DEPENDENT_SHAPE_REPRESENTATION(#144,#10388);
#205=CONTEXT_DEPENDENT_SHAPE_REPRESENTATION(#145,#10389);
#206=CONTEXT_DEPENDENT_SHAPE_REPRESENTATION(#146,#10390);
#207=CONTEXT_DEPENDENT_SHAPE_REPRESENTATION(#147,#10391);
#208=CONTEXT_DEPENDENT_SHAPE_REPRESENTATION(#148,#10392);
#209=CONTEXT_DEPENDENT_SHAPE_REPRESENTATION(#149,#10393);
#210=CONTEXT_DEPENDENT_SHAPE_REPRESENTATION(#150,#10394);
#211=CONTEXT_DEPENDENT_SHAPE_REPRESENTATION(#151,#10395);
#212=CONTEXT_DEPENDENT_SHAPE_REPRESENTATION(#152,#10396);
#213=CONTEXT_DEPENDENT_SHAPE_REPRESENTATION(#153,#10397);
#214=CONTEXT_DEPENDENT_SHAPE_REPRESENTATION(#154,#10398);
#215=CONTEXT_DEPENDENT_SHAPE_REPRESENTATION(#155,#10399);
#216=CONTEXT_DEPENDENT_SHAPE_REPRESENTATION(#156,#10400);
#217=CONTEXT_DEPENDENT_SHAPE_REPRESENTATION(#157,#10401);
#218=CONTEXT_DEPENDENT_SHAPE_REPRESENTATION(#158,#10402);
#219=CONTEXT_DEPENDENT_SHAPE_REPRESENTATION(#159,#10403);
#220=NEXT_ASSEMBLY_USAGE_OCCURRENCE('Steel sleeve:1','Steel sleeve:1',
'Steel sleeve:1',#10462,#10463,'Steel sleeve:1');
#221=NEXT_ASSEMBLY_USAGE_OCCURRENCE('Ball retainer (plastic):1',
'Ball retainer (plastic):1','Ball retainer (plastic):1',#10462,#10464,
'Ball retainer (plastic):1');
#222=NEXT_ASSEMBLY_USAGE_OCCURRENCE('Body:1','Body:1','Body:1',#10466,#10467,
'Body:1');
#223=NEXT_ASSEMBLY_USAGE_OCCURRENCE('Release collar:1',
'Release collar:1','Release collar:1',#10466,#10468,'Release collar:1');
#224=NEXT_ASSEMBLY_USAGE_OCCURRENCE('Mounting plate:1',
'Mounting plate:1','Mounting plate:1',#10443,#10444,'Mounting plate:1');
#225=NEXT_ASSEMBLY_USAGE_OCCURRENCE('Foot strip:1','Foot strip:1',
'Foot strip:1',#10443,#10445,'Foot strip:1');
#226=NEXT_ASSEMBLY_USAGE_OCCURRENCE('Foot strip (1):1',
'Foot strip (1):1','Foot strip (1):1',#10443,#10446,'Foot strip (1):1');
#227=NEXT_ASSEMBLY_USAGE_OCCURRENCE('Guide body:1','Guide body:1',
'Guide body:1',#10443,#10447,'Guide body:1');
#228=NEXT_ASSEMBLY_USAGE_OCCURRENCE('Guide cap:1','Guide cap:1',
'Guide cap:1',#10443,#10448,'Guide cap:1');
#229=NEXT_ASSEMBLY_USAGE_OCCURRENCE('Retracted stop sleeve:1',
'Retracted stop sleeve:1','Retracted stop sleeve:1',#10443,#10449,
'Retracted stop sleeve:1');
#230=NEXT_ASSEMBLY_USAGE_OCCURRENCE('Installed return spring:1',
'Installed return spring:1','Installed return spring:1',#10443,#10450,
'Installed return spring:1');
#231=NEXT_ASSEMBLY_USAGE_OCCURRENCE('Extended travel stop frame:1',
'Extended travel stop frame:1','Extended travel stop frame:1',#10443,#10451,
'Extended travel stop frame:1');
#232=NEXT_ASSEMBLY_USAGE_OCCURRENCE('Cylinder bottom cap:1',
'Cylinder bottom cap:1','Cylinder bottom cap:1',#10443,#10452,
'Cylinder bottom cap:1');
#233=NEXT_ASSEMBLY_USAGE_OCCURRENCE('Barrel gasket:1','Barrel gasket:1',
'Barrel gasket:1',#10443,#10453,'Barrel gasket:1');
#234=NEXT_ASSEMBLY_USAGE_OCCURRENCE('Cylinder top cap:1',
'Cylinder top cap:1','Cylinder top cap:1',#10443,#10454,
'Cylinder top cap:1');
#235=NEXT_ASSEMBLY_USAGE_OCCURRENCE('Barrel gasket (1):1',
'Barrel gasket (1):1','Barrel gasket (1):1',#10443,#10455,
'Barrel gasket (1):1');
#236=NEXT_ASSEMBLY_USAGE_OCCURRENCE('Cylinder tube:1','Cylinder tube:1',
'Cylinder tube:1',#10443,#10456,'Cylinder tube:1');
#237=NEXT_ASSEMBLY_USAGE_OCCURRENCE('Rod seal envelope:1',
'Rod seal envelope:1','Rod seal envelope:1',#10443,#10457,
'Rod seal envelope:1');
#238=NEXT_ASSEMBLY_USAGE_OCCURRENCE('M5 tie rod:1','M5 tie rod:1',
'M5 tie rod:1',#10443,#10458,'M5 tie rod:1');
#239=NEXT_ASSEMBLY_USAGE_OCCURRENCE('M5 tie rod (1):1',
'M5 tie rod (1):1','M5 tie rod (1):1',#10443,#10459,'M5 tie rod (1):1');
#240=NEXT_ASSEMBLY_USAGE_OCCURRENCE('M5 tie rod (2):1',
'M5 tie rod (2):1','M5 tie rod (2):1',#10443,#10460,'M5 tie rod (2):1');
#241=NEXT_ASSEMBLY_USAGE_OCCURRENCE('M5 tie rod (3):1',
'M5 tie rod (3):1','M5 tie rod (3):1',#10443,#10461,'M5 tie rod (3):1');
#242=NEXT_ASSEMBLY_USAGE_OCCURRENCE(
'Linear Ball Bushing - 12 x 21 x 30 mm:2',
'Linear Ball Bushing - 12 x 21 x 30 mm:2',
'Linear Ball Bushing - 12 x 21 x 30 mm:2',#10443,#10462,
'Linear Ball Bushing - 12 x 21 x 30 mm:2');
#243=NEXT_ASSEMBLY_USAGE_OCCURRENCE('Cap Screw - M5x20:2',
'Cap Screw - M5x20:2','Cap Screw - M5x20:2',#10443,#10465,
'Cap Screw - M5x20:2');
#244=NEXT_ASSEMBLY_USAGE_OCCURRENCE('Cap Screw - M5x20:3',
'Cap Screw - M5x20:3','Cap Screw - M5x20:3',#10443,#10465,
'Cap Screw - M5x20:3');
#245=NEXT_ASSEMBLY_USAGE_OCCURRENCE('Cap Screw - M5x20:4',
'Cap Screw - M5x20:4','Cap Screw - M5x20:4',#10443,#10465,
'Cap Screw - M5x20:4');
#246=NEXT_ASSEMBLY_USAGE_OCCURRENCE('Cap Screw - M5x20:5',
'Cap Screw - M5x20:5','Cap Screw - M5x20:5',#10443,#10465,
'Cap Screw - M5x20:5');
#247=NEXT_ASSEMBLY_USAGE_OCCURRENCE('Cap Screw - M4x16:2',
'Cap Screw - M4x16:2','Cap Screw - M4x16:2',#10443,#10478,
'Cap Screw - M4x16:2');
#248=NEXT_ASSEMBLY_USAGE_OCCURRENCE('Cap Screw - M4x16:3',
'Cap Screw - M4x16:3','Cap Screw - M4x16:3',#10443,#10478,
'Cap Screw - M4x16:3');
#249=NEXT_ASSEMBLY_USAGE_OCCURRENCE('Cap Screw - M4x16:4',
'Cap Screw - M4x16:4','Cap Screw - M4x16:4',#10443,#10478,
'Cap Screw - M4x16:4');
#250=NEXT_ASSEMBLY_USAGE_OCCURRENCE('Cap Screw - M4x16:5',
'Cap Screw - M4x16:5','Cap Screw - M4x16:5',#10443,#10478,
'Cap Screw - M4x16:5');
#251=NEXT_ASSEMBLY_USAGE_OCCURRENCE('Cap Screw - M5x20:6',
'Cap Screw - M5x20:6','Cap Screw - M5x20:6',#10443,#10465,
'Cap Screw - M5x20:6');
#252=NEXT_ASSEMBLY_USAGE_OCCURRENCE(
'Push-In Tube Fitting - 6 mm Tube, 1-8 Inch Tapered Pipe Thread:2',
'Push-In Tube Fitting - 6 mm Tube, 1-8 Inch Tapered Pipe Thread:2',
'Push-In Tube Fitting - 6 mm Tube, 1-8 Inch Tapered Pipe Thread:2',#10443,
#10466,
'Push-In Tube Fitting - 6 mm Tube, 1-8 Inch Tapered Pipe Thread:2');
#253=NEXT_ASSEMBLY_USAGE_OCCURRENCE(
'Push-In Tube Fitting - 6 mm Tube, 1-8 Inch Tapered Pipe Thread:3',
'Push-In Tube Fitting - 6 mm Tube, 1-8 Inch Tapered Pipe Thread:3',
'Push-In Tube Fitting - 6 mm Tube, 1-8 Inch Tapered Pipe Thread:3',#10443,
#10466,
'Push-In Tube Fitting - 6 mm Tube, 1-8 Inch Tapered Pipe Thread:3');
#254=NEXT_ASSEMBLY_USAGE_OCCURRENCE('Flat Washer - M5:2',
'Flat Washer - M5:2','Flat Washer - M5:2',#10443,#10469,
'Flat Washer - M5:2');
#255=NEXT_ASSEMBLY_USAGE_OCCURRENCE('Hex Nut - M5:2','Hex Nut - M5:2',
'Hex Nut - M5:2',#10443,#10470,'Hex Nut - M5:2');
#256=NEXT_ASSEMBLY_USAGE_OCCURRENCE('Flat Washer - M5:3',
'Flat Washer - M5:3','Flat Washer - M5:3',#10443,#10469,
'Flat Washer - M5:3');
#257=NEXT_ASSEMBLY_USAGE_OCCURRENCE('Hex Nut - M5:3','Hex Nut - M5:3',
'Hex Nut - M5:3',#10443,#10470,'Hex Nut - M5:3');
#258=NEXT_ASSEMBLY_USAGE_OCCURRENCE('Flat Washer - M5:4',
'Flat Washer - M5:4','Flat Washer - M5:4',#10443,#10469,
'Flat Washer - M5:4');
#259=NEXT_ASSEMBLY_USAGE_OCCURRENCE('Hex Nut - M5:4','Hex Nut - M5:4',
'Hex Nut - M5:4',#10443,#10470,'Hex Nut - M5:4');
#260=NEXT_ASSEMBLY_USAGE_OCCURRENCE('Flat Washer - M5:5',
'Flat Washer - M5:5','Flat Washer - M5:5',#10443,#10469,
'Flat Washer - M5:5');
#261=NEXT_ASSEMBLY_USAGE_OCCURRENCE('Hex Nut - M5:5','Hex Nut - M5:5',
'Hex Nut - M5:5',#10443,#10470,'Hex Nut - M5:5');
#262=NEXT_ASSEMBLY_USAGE_OCCURRENCE('Flat Washer - M5:6',
'Flat Washer - M5:6','Flat Washer - M5:6',#10443,#10469,
'Flat Washer - M5:6');
#263=NEXT_ASSEMBLY_USAGE_OCCURRENCE('Hex Nut - M5:6','Hex Nut - M5:6',
'Hex Nut - M5:6',#10443,#10470,'Hex Nut - M5:6');
#264=NEXT_ASSEMBLY_USAGE_OCCURRENCE('Flat Washer - M5:7',
'Flat Washer - M5:7','Flat Washer - M5:7',#10443,#10469,
'Flat Washer - M5:7');
#265=NEXT_ASSEMBLY_USAGE_OCCURRENCE('Hex Nut - M5:7','Hex Nut - M5:7',
'Hex Nut - M5:7',#10443,#10470,'Hex Nut - M5:7');
#266=NEXT_ASSEMBLY_USAGE_OCCURRENCE('Flat Washer - M5:8',
'Flat Washer - M5:8','Flat Washer - M5:8',#10443,#10469,
'Flat Washer - M5:8');
#267=NEXT_ASSEMBLY_USAGE_OCCURRENCE('Hex Nut - M5:8','Hex Nut - M5:8',
'Hex Nut - M5:8',#10443,#10470,'Hex Nut - M5:8');
#268=NEXT_ASSEMBLY_USAGE_OCCURRENCE('Flat Washer - M5:9',
'Flat Washer - M5:9','Flat Washer - M5:9',#10443,#10469,
'Flat Washer - M5:9');
#269=NEXT_ASSEMBLY_USAGE_OCCURRENCE('Hex Nut - M5:9','Hex Nut - M5:9',
'Hex Nut - M5:9',#10443,#10470,'Hex Nut - M5:9');
#270=NEXT_ASSEMBLY_USAGE_OCCURRENCE('Stop blade:1','Stop blade:1',
'Stop blade:1',#10471,#10472,'Stop blade:1');
#271=NEXT_ASSEMBLY_USAGE_OCCURRENCE('Piston rod:1','Piston rod:1',
'Piston rod:1',#10471,#10473,'Piston rod:1');
#272=NEXT_ASSEMBLY_USAGE_OCCURRENCE('Piston:1','Piston:1','Piston:1',#10471,
#10474,'Piston:1');
#273=NEXT_ASSEMBLY_USAGE_OCCURRENCE('Piston seal envelope:1',
'Piston seal envelope:1','Piston seal envelope:1',#10471,#10475,
'Piston seal envelope:1');
#274=NEXT_ASSEMBLY_USAGE_OCCURRENCE('100 mm guide shaft:2',
'100 mm guide shaft:2','100 mm guide shaft:2',#10471,#10476,
'100 mm guide shaft:2');
#275=NEXT_ASSEMBLY_USAGE_OCCURRENCE('M4x4 shaft screw:2',
'M4x4 shaft screw:2','M4x4 shaft screw:2',#10471,#10477,
'M4x4 shaft screw:2');
#276=NEXT_ASSEMBLY_USAGE_OCCURRENCE('Cap Screw - M4x16:6',
'Cap Screw - M4x16:6','Cap Screw - M4x16:6',#10471,#10478,
'Cap Screw - M4x16:6');
#277=NEXT_ASSEMBLY_USAGE_OCCURRENCE('Cap Screw - M4x16:7',
'Cap Screw - M4x16:7','Cap Screw - M4x16:7',#10471,#10478,
'Cap Screw - M4x16:7');
#278=NEXT_ASSEMBLY_USAGE_OCCURRENCE('Mounting body and return spring:1',
'Mounting body and return spring:1','Mounting body and return spring:1',
#10442,#10443,'Mounting body and return spring:1');
#279=NEXT_ASSEMBLY_USAGE_OCCURRENCE('Blade, shaft and piston:1',
'Blade, shaft and piston:1','Blade, shaft and piston:1',#10442,#10471,
'Blade, shaft and piston:1');
#280=B_SPLINE_CURVE_WITH_KNOTS('',3,(#8824,#8825,#8826,#8827,#8828,#8829,
#8830,#8831,#8832,#8833,#8834,#8835,#8836,#8837,#8838,#8839,#8840,#8841,
#8842,#8843,#8844,#8845,#8846,#8847,#8848,#8849,#8850,#8851,#8852,#8853,
#8854,#8855,#8856,#8857,#8858,#8859,#8860,#8861,#8862,#8863,#8864,#8865,
#8866,#8867,#8868,#8869,#8870,#8871,#8872,#8873,#8874,#8875,#8876,#8877,
#8878,#8879,#8880,#8881,#8882,#8883,#8884,#8885,#8886,#8887,#8888,#8889,
#8890,#8891,#8892,#8893,#8894,#8895,#8896,#8897,#8898,#8899),
 .UNSPECIFIED.,.F.,.F.,(4,1,1,1,1,1,1,1,1,1,1,1,1,1,1,1,1,1,1,1,1,1,1,1,
1,1,1,1,1,1,1,1,1,1,1,1,1,1,1,1,1,1,1,1,1,1,1,1,1,1,1,1,1,1,1,1,1,1,1,1,
1,1,1,1,1,1,1,1,1,1,1,1,1,4),(0.,0.0178571428571429,0.0357142857142857,
0.0535714285714286,0.0714285714285714,0.0892857142857143,0.107142857142857,
0.125,0.127232142857143,0.129464285714286,0.133928571428571,0.138392857142857,
0.142857142857143,0.158730158730159,0.174603174603175,0.19047619047619,
0.202380952380952,0.214285714285714,0.226190476190476,0.238095238095238,
0.25,0.261904761904762,0.267857142857143,0.273809523809524,0.285714285714286,
0.297619047619048,0.30952380952381,0.321428571428571,0.333333333333333,
0.349206349206349,0.365079365079365,0.373015873015873,0.380952380952381,
0.396825396825397,0.412698412698413,0.428571428571429,0.446428571428571,
0.464285714285714,0.476190476190476,0.488095238095238,0.5,0.517857142857143,
0.535714285714286,0.553571428571429,0.571428571428571,0.589285714285714,
0.607142857142857,0.625,0.642857142857143,0.651785714285714,0.660714285714286,
0.678571428571428,0.696428571428571,0.714285714285714,0.726190476190476,
0.738095238095238,0.75,0.761904761904762,0.773809523809524,0.785714285714286,
0.797619047619047,0.809523809523809,0.821428571428571,0.833333333333333,
0.845238095238095,0.857142857142857,0.875,0.892857142857143,0.910714285714286,
0.928571428571429,0.946428571428571,0.964285714285714,0.982142857142857,
1.),.UNSPECIFIED.);
#281=B_SPLINE_CURVE_WITH_KNOTS('',3,(#8964,#8965,#8966,#8967,#8968,#8969,
#8970,#8971,#8972,#8973,#8974,#8975,#8976,#8977,#8978,#8979,#8980,#8981,
#8982,#8983,#8984,#8985,#8986,#8987,#8988,#8989),.UNSPECIFIED.,.F.,.F.,
(4,2,2,2,2,2,2,2,2,2,2,2,4),(4.86208093968474,5.16603148466369,5.46998202964264,
5.77379160212428,6.07760117460592,6.38141074708757,6.68522031956921,6.98917086454816,
7.29312140952711,7.59707195450606,7.90102249948501,8.20483207196665,8.50864164444829),
 .UNSPECIFIED.);
#282=B_SPLINE_CURVE_WITH_KNOTS('',3,(#8999,#9000,#9001,#9002,#9003,#9004,
#9005,#9006,#9007,#9008,#9009,#9010,#9011,#9012,#9013,#9014,#9015,#9016),
 .UNSPECIFIED.,.F.,.F.,(4,2,2,2,2,2,2,2,4),(0.,0.0755590511780388,0.151118102356078,
0.226672919608918,0.302227736861757,0.377782554114597,0.453337371367437,
0.528896422545476,0.604455473723515),.UNSPECIFIED.);
#283=B_SPLINE_CURVE_WITH_KNOTS('',3,(#9033,#9034,#9035,#9036,#9037,#9038,
#9039,#9040,#9041,#9042),.UNSPECIFIED.,.F.,.F.,(4,2,2,2,4),(3.64656070476355,
3.9503702772452,4.25417984972684,4.55813039470579,4.86208093968474),
 .UNSPECIFIED.);
#284=B_SPLINE_CURVE_WITH_KNOTS('',3,(#9117,#9118,#9119,#9120,#9121,#9122,
#9123,#9124),.UNSPECIFIED.,.F.,.F.,(4,2,2,4),(-0.590204267533974,-0.538821839180455,
-0.508604823357851,-0.478387807535247),.UNSPECIFIED.);
#285=B_SPLINE_CURVE_WITH_KNOTS('',3,(#9128,#9129,#9130,#9131,#9132,#9133,
#9134,#9135,#9136,#9137,#9138,#9139,#9140,#9141,#9142,#9143,#9144,#9145,
#9146,#9147,#9148,#9149,#9150,#9151,#9152,#9153,#9154,#9155,#9156),
 .UNSPECIFIED.,.F.,.F.,(4,2,2,2,2,2,2,2,2,2,3,2,2,4),(-0.478387807535247,
-0.448170791712642,-0.417953775890038,-0.357519744244829,-0.298356824006226,
-0.239193903767623,-0.180030983529021,-0.120868063290418,-0.0604340316452091,
-0.0302170158226045,1.11022302462516E-16,0.0302170158226046,0.0604340316452092,
0.111816459998729),.UNSPECIFIED.);
#286=B_SPLINE_CURVE_WITH_KNOTS('',3,(#9177,#9178,#9179,#9180,#9181,#9182,
#9183,#9184,#9185,#9186,#9187,#9188,#9189,#9190,#9191,#9192,#9193,#9194,
#9195,#9196,#9197,#9198,#9199,#9200,#9201,#9202,#9203,#9204,#9205,#9206,
#9207,#9208,#9209,#9210),.UNSPECIFIED.,.T.,.F.,(4,2,2,2,2,2,2,2,2,2,2,2,
2,2,2,2,4),(0.,0.303950544978949,0.607901089957899,0.911710662439542,1.21552023492119,
1.51932980740283,1.82313937988447,2.12708992486342,2.43104046984237,2.73499101482132,
3.03894155980027,3.34275113228191,3.64656070476356,3.9503702772452,4.25417984972684,
4.55813039470579,4.86208093968474),.UNSPECIFIED.);
#287=B_SPLINE_CURVE_WITH_KNOTS('',3,(#9812,#9813,#9814,#9815,#9816,#9817,
#9818,#9819,#9820,#9821,#9822,#9823,#9824,#9825),.UNSPECIFIED.,.F.,.F.,
(4,2,2,2,2,2,4),(0.598759573717651,0.624973342427789,0.687463163426141,
0.749952984424493,0.812442805422845,0.874932626421197,0.901146395131335),
 .UNSPECIFIED.);
#288=B_SPLINE_CURVE_WITH_KNOTS('',3,(#9829,#9830,#9831,#9832,#9833,#9834,
#9835,#9836),.UNSPECIFIED.,.F.,.F.,(4,2,2,4),(0.249984328141498,0.31247414913985,
0.374963970138202,0.401177738848337),.UNSPECIFIED.);
#289=B_SPLINE_CURVE_WITH_KNOTS('',3,(#9840,#9841,#9842,#9843,#9844,#9845,
#9846,#9847,#9848,#9849,#9850,#9851,#9852,#9853,#9854,#9855,#9856,#9857,
#9858,#9859,#9860,#9861,#9862,#9863,#9864,#9865),.UNSPECIFIED.,.F.,.F.,
(4,2,2,2,2,2,2,2,2,2,2,2,4),(0.,0.0622766332261793,0.124553266452359,0.186828302721277,
0.249103338990195,0.311378375259114,0.373653411528032,0.435930044754212,
0.498206677980391,0.56048331120657,0.62275994443275,0.685034980701668,0.747310016970586),
 .UNSPECIFIED.);
#290=B_SPLINE_CURVE_WITH_KNOTS('',3,(#9866,#9867,#9868,#9869,#9870,#9871,
#9872,#9873,#9874,#9875),.UNSPECIFIED.,.F.,.F.,(4,2,2,2,4),(0.747310016970586,
0.809585053239505,0.871860089508423,0.934136722734602,0.996413355960782),
 .UNSPECIFIED.);
#291=B_SPLINE_CURVE_WITH_KNOTS('',3,(#9876,#9877,#9878,#9879,#9880,#9881,
#9882,#9883),.UNSPECIFIED.,.F.,.F.,(4,2,2,4),(0.0987909174346565,0.125004686144793,
0.187494507143146,0.249984328141498),.UNSPECIFIED.);
#292=B_SPLINE_SURFACE_WITH_KNOTS('',3,3,((#8061,#8062,#8063,#8064,#8065,
#8066,#8067,#8068,#8069,#8070,#8071,#8072,#8073,#8074,#8075,#8076,#8077,
#8078,#8079,#8080,#8081,#8082,#8083,#8084,#8085,#8086,#8087,#8088,#8089,
#8090,#8091,#8092,#8093,#8094,#8095,#8096,#8097,#8098,#8099,#8100,#8101,
#8102,#8103,#8104,#8105,#8106,#8107,#8108,#8109,#8110,#8111,#8112,#8113,
#8114,#8115,#8116,#8117,#8118,#8119,#8120,#8121,#8122,#8123,#8124,#8125,
#8126,#8127,#8128,#8129,#8130,#8131,#8132,#8133,#8134,#8135,#8136),(#8137,
#8138,#8139,#8140,#8141,#8142,#8143,#8144,#8145,#8146,#8147,#8148,#8149,
#8150,#8151,#8152,#8153,#8154,#8155,#8156,#8157,#8158,#8159,#8160,#8161,
#8162,#8163,#8164,#8165,#8166,#8167,#8168,#8169,#8170,#8171,#8172,#8173,
#8174,#8175,#8176,#8177,#8178,#8179,#8180,#8181,#8182,#8183,#8184,#8185,
#8186,#8187,#8188,#8189,#8190,#8191,#8192,#8193,#8194,#8195,#8196,#8197,
#8198,#8199,#8200,#8201,#8202,#8203,#8204,#8205,#8206,#8207,#8208,#8209,
#8210,#8211,#8212),(#8213,#8214,#8215,#8216,#8217,#8218,#8219,#8220,#8221,
#8222,#8223,#8224,#8225,#8226,#8227,#8228,#8229,#8230,#8231,#8232,#8233,
#8234,#8235,#8236,#8237,#8238,#8239,#8240,#8241,#8242,#8243,#8244,#8245,
#8246,#8247,#8248,#8249,#8250,#8251,#8252,#8253,#8254,#8255,#8256,#8257,
#8258,#8259,#8260,#8261,#8262,#8263,#8264,#8265,#8266,#8267,#8268,#8269,
#8270,#8271,#8272,#8273,#8274,#8275,#8276,#8277,#8278,#8279,#8280,#8281,
#8282,#8283,#8284,#8285,#8286,#8287,#8288),(#8289,#8290,#8291,#8292,#8293,
#8294,#8295,#8296,#8297,#8298,#8299,#8300,#8301,#8302,#8303,#8304,#8305,
#8306,#8307,#8308,#8309,#8310,#8311,#8312,#8313,#8314,#8315,#8316,#8317,
#8318,#8319,#8320,#8321,#8322,#8323,#8324,#8325,#8326,#8327,#8328,#8329,
#8330,#8331,#8332,#8333,#8334,#8335,#8336,#8337,#8338,#8339,#8340,#8341,
#8342,#8343,#8344,#8345,#8346,#8347,#8348,#8349,#8350,#8351,#8352,#8353,
#8354,#8355,#8356,#8357,#8358,#8359,#8360,#8361,#8362,#8363,#8364),(#8365,
#8366,#8367,#8368,#8369,#8370,#8371,#8372,#8373,#8374,#8375,#8376,#8377,
#8378,#8379,#8380,#8381,#8382,#8383,#8384,#8385,#8386,#8387,#8388,#8389,
#8390,#8391,#8392,#8393,#8394,#8395,#8396,#8397,#8398,#8399,#8400,#8401,
#8402,#8403,#8404,#8405,#8406,#8407,#8408,#8409,#8410,#8411,#8412,#8413,
#8414,#8415,#8416,#8417,#8418,#8419,#8420,#8421,#8422,#8423,#8424,#8425,
#8426,#8427,#8428,#8429,#8430,#8431,#8432,#8433,#8434,#8435,#8436,#8437,
#8438,#8439,#8440),(#8441,#8442,#8443,#8444,#8445,#8446,#8447,#8448,#8449,
#8450,#8451,#8452,#8453,#8454,#8455,#8456,#8457,#8458,#8459,#8460,#8461,
#8462,#8463,#8464,#8465,#8466,#8467,#8468,#8469,#8470,#8471,#8472,#8473,
#8474,#8475,#8476,#8477,#8478,#8479,#8480,#8481,#8482,#8483,#8484,#8485,
#8486,#8487,#8488,#8489,#8490,#8491,#8492,#8493,#8494,#8495,#8496,#8497,
#8498,#8499,#8500,#8501,#8502,#8503,#8504,#8505,#8506,#8507,#8508,#8509,
#8510,#8511,#8512,#8513,#8514,#8515,#8516),(#8517,#8518,#8519,#8520,#8521,
#8522,#8523,#8524,#8525,#8526,#8527,#8528,#8529,#8530,#8531,#8532,#8533,
#8534,#8535,#8536,#8537,#8538,#8539,#8540,#8541,#8542,#8543,#8544,#8545,
#8546,#8547,#8548,#8549,#8550,#8551,#8552,#8553,#8554,#8555,#8556,#8557,
#8558,#8559,#8560,#8561,#8562,#8563,#8564,#8565,#8566,#8567,#8568,#8569,
#8570,#8571,#8572,#8573,#8574,#8575,#8576,#8577,#8578,#8579,#8580,#8581,
#8582,#8583,#8584,#8585,#8586,#8587,#8588,#8589,#8590,#8591,#8592),(#8593,
#8594,#8595,#8596,#8597,#8598,#8599,#8600,#8601,#8602,#8603,#8604,#8605,
#8606,#8607,#8608,#8609,#8610,#8611,#8612,#8613,#8614,#8615,#8616,#8617,
#8618,#8619,#8620,#8621,#8622,#8623,#8624,#8625,#8626,#8627,#8628,#8629,
#8630,#8631,#8632,#8633,#8634,#8635,#8636,#8637,#8638,#8639,#8640,#8641,
#8642,#8643,#8644,#8645,#8646,#8647,#8648,#8649,#8650,#8651,#8652,#8653,
#8654,#8655,#8656,#8657,#8658,#8659,#8660,#8661,#8662,#8663,#8664,#8665,
#8666,#8667,#8668),(#8669,#8670,#8671,#8672,#8673,#8674,#8675,#8676,#8677,
#8678,#8679,#8680,#8681,#8682,#8683,#8684,#8685,#8686,#8687,#8688,#8689,
#8690,#8691,#8692,#8693,#8694,#8695,#8696,#8697,#8698,#8699,#8700,#8701,
#8702,#8703,#8704,#8705,#8706,#8707,#8708,#8709,#8710,#8711,#8712,#8713,
#8714,#8715,#8716,#8717,#8718,#8719,#8720,#8721,#8722,#8723,#8724,#8725,
#8726,#8727,#8728,#8729,#8730,#8731,#8732,#8733,#8734,#8735,#8736,#8737,
#8738,#8739,#8740,#8741,#8742,#8743,#8744),(#8745,#8746,#8747,#8748,#8749,
#8750,#8751,#8752,#8753,#8754,#8755,#8756,#8757,#8758,#8759,#8760,#8761,
#8762,#8763,#8764,#8765,#8766,#8767,#8768,#8769,#8770,#8771,#8772,#8773,
#8774,#8775,#8776,#8777,#8778,#8779,#8780,#8781,#8782,#8783,#8784,#8785,
#8786,#8787,#8788,#8789,#8790,#8791,#8792,#8793,#8794,#8795,#8796,#8797,
#8798,#8799,#8800,#8801,#8802,#8803,#8804,#8805,#8806,#8807,#8808,#8809,
#8810,#8811,#8812,#8813,#8814,#8815,#8816,#8817,#8818,#8819,#8820)),
 .UNSPECIFIED.,.T.,.F.,.F.,(4,1,1,1,1,1,1,4),(4,1,1,1,1,1,1,1,1,1,1,1,1,
1,1,1,1,1,1,1,1,1,1,1,1,1,1,1,1,1,1,1,1,1,1,1,1,1,1,1,1,1,1,1,1,1,1,1,1,
1,1,1,1,1,1,1,1,1,1,1,1,1,1,1,1,1,1,1,1,1,1,1,1,4),(-3.14159265358979,-2.24399475256414,
-1.34639685153848,-0.448798950512828,0.448798950512828,1.34639685153848,
2.24399475256414,3.14159265358979),(0.,0.0178571428571429,0.0357142857142857,
0.0535714285714286,0.0714285714285714,0.0892857142857143,0.107142857142857,
0.125,0.127232142857143,0.129464285714286,0.133928571428571,0.138392857142857,
0.142857142857143,0.158730158730159,0.174603174603175,0.19047619047619,
0.202380952380952,0.214285714285714,0.226190476190476,0.238095238095238,
0.25,0.261904761904762,0.267857142857143,0.273809523809524,0.285714285714286,
0.297619047619048,0.30952380952381,0.321428571428571,0.333333333333333,
0.349206349206349,0.365079365079365,0.373015873015873,0.380952380952381,
0.396825396825397,0.412698412698413,0.428571428571429,0.446428571428571,
0.464285714285714,0.476190476190476,0.488095238095238,0.5,0.517857142857143,
0.535714285714286,0.553571428571429,0.571428571428571,0.589285714285714,
0.607142857142857,0.625,0.642857142857143,0.651785714285714,0.660714285714286,
0.678571428571428,0.696428571428571,0.714285714285714,0.726190476190476,
0.738095238095238,0.75,0.761904761904762,0.773809523809524,0.785714285714286,
0.797619047619047,0.809523809523809,0.821428571428571,0.833333333333333,
0.845238095238095,0.857142857142857,0.875,0.892857142857143,0.910714285714286,
0.928571428571429,0.946428571428571,0.964285714285714,0.982142857142857,
1.),.UNSPECIFIED.);
#293=SHAPE_REPRESENTATION_RELATIONSHIP('SRR','None',#10406,#325);
#294=SHAPE_REPRESENTATION_RELATIONSHIP('SRR','None',#10407,#326);
#295=SHAPE_REPRESENTATION_RELATIONSHIP('SRR','None',#10408,#327);
#296=SHAPE_REPRESENTATION_RELATIONSHIP('SRR','None',#10409,#328);
#297=SHAPE_REPRESENTATION_RELATIONSHIP('SRR','None',#10410,#329);
#298=SHAPE_REPRESENTATION_RELATIONSHIP('SRR','None',#10411,#330);
#299=SHAPE_REPRESENTATION_RELATIONSHIP('SRR','None',#10412,#331);
#300=SHAPE_REPRESENTATION_RELATIONSHIP('SRR','None',#10413,#332);
#301=SHAPE_REPRESENTATION_RELATIONSHIP('SRR','None',#10414,#333);
#302=SHAPE_REPRESENTATION_RELATIONSHIP('SRR','None',#10415,#334);
#303=SHAPE_REPRESENTATION_RELATIONSHIP('SRR','None',#10416,#335);
#304=SHAPE_REPRESENTATION_RELATIONSHIP('SRR','None',#10417,#336);
#305=SHAPE_REPRESENTATION_RELATIONSHIP('SRR','None',#10418,#337);
#306=SHAPE_REPRESENTATION_RELATIONSHIP('SRR','None',#10419,#338);
#307=SHAPE_REPRESENTATION_RELATIONSHIP('SRR','None',#10420,#339);
#308=SHAPE_REPRESENTATION_RELATIONSHIP('SRR','None',#10421,#340);
#309=SHAPE_REPRESENTATION_RELATIONSHIP('SRR','None',#10422,#341);
#310=SHAPE_REPRESENTATION_RELATIONSHIP('SRR','None',#10423,#342);
#311=SHAPE_REPRESENTATION_RELATIONSHIP('SRR','None',#10425,#343);
#312=SHAPE_REPRESENTATION_RELATIONSHIP('SRR','None',#10426,#344);
#313=SHAPE_REPRESENTATION_RELATIONSHIP('SRR','None',#10427,#345);
#314=SHAPE_REPRESENTATION_RELATIONSHIP('SRR','None',#10429,#346);
#315=SHAPE_REPRESENTATION_RELATIONSHIP('SRR','None',#10430,#347);
#316=SHAPE_REPRESENTATION_RELATIONSHIP('SRR','None',#10431,#348);
#317=SHAPE_REPRESENTATION_RELATIONSHIP('SRR','None',#10432,#349);
#318=SHAPE_REPRESENTATION_RELATIONSHIP('SRR','None',#10434,#350);
#319=SHAPE_REPRESENTATION_RELATIONSHIP('SRR','None',#10435,#351);
#320=SHAPE_REPRESENTATION_RELATIONSHIP('SRR','None',#10436,#352);
#321=SHAPE_REPRESENTATION_RELATIONSHIP('SRR','None',#10437,#353);
#322=SHAPE_REPRESENTATION_RELATIONSHIP('SRR','None',#10438,#354);
#323=SHAPE_REPRESENTATION_RELATIONSHIP('SRR','None',#10439,#355);
#324=SHAPE_REPRESENTATION_RELATIONSHIP('SRR','None',#10440,#356);
#325=ADVANCED_BREP_SHAPE_REPRESENTATION('',(#389),#10230);
#326=ADVANCED_BREP_SHAPE_REPRESENTATION('',(#390),#10231);
#327=ADVANCED_BREP_SHAPE_REPRESENTATION('',(#391),#10232);
#328=ADVANCED_BREP_SHAPE_REPRESENTATION('',(#392),#10233);
#329=ADVANCED_BREP_SHAPE_REPRESENTATION('',(#393),#10234);
#330=ADVANCED_BREP_SHAPE_REPRESENTATION('',(#394),#10235);
#331=ADVANCED_BREP_SHAPE_REPRESENTATION('',(#395),#10236);
#332=ADVANCED_BREP_SHAPE_REPRESENTATION('',(#396),#10237);
#333=ADVANCED_BREP_SHAPE_REPRESENTATION('',(#397),#10238);
#334=ADVANCED_BREP_SHAPE_REPRESENTATION('',(#398),#10239);
#335=ADVANCED_BREP_SHAPE_REPRESENTATION('',(#399),#10240);
#336=ADVANCED_BREP_SHAPE_REPRESENTATION('',(#400),#10241);
#337=ADVANCED_BREP_SHAPE_REPRESENTATION('',(#401),#10242);
#338=ADVANCED_BREP_SHAPE_REPRESENTATION('',(#402),#10243);
#339=ADVANCED_BREP_SHAPE_REPRESENTATION('',(#403),#10244);
#340=ADVANCED_BREP_SHAPE_REPRESENTATION('',(#404),#10245);
#341=ADVANCED_BREP_SHAPE_REPRESENTATION('',(#405),#10246);
#342=ADVANCED_BREP_SHAPE_REPRESENTATION('',(#406),#10247);
#343=ADVANCED_BREP_SHAPE_REPRESENTATION('',(#407),#10249);
#344=ADVANCED_BREP_SHAPE_REPRESENTATION('',(#408),#10250);
#345=ADVANCED_BREP_SHAPE_REPRESENTATION('',(#38),#10251);
#346=ADVANCED_BREP_SHAPE_REPRESENTATION('',(#409),#10253);
#347=ADVANCED_BREP_SHAPE_REPRESENTATION('',(#410),#10254);
#348=ADVANCED_BREP_SHAPE_REPRESENTATION('',(#411),#10255);
#349=ADVANCED_BREP_SHAPE_REPRESENTATION('',(#412),#10256);
#350=ADVANCED_BREP_SHAPE_REPRESENTATION('',(#413),#10258);
#351=ADVANCED_BREP_SHAPE_REPRESENTATION('',(#414),#10259);
#352=ADVANCED_BREP_SHAPE_REPRESENTATION('',(#415),#10260);
#353=ADVANCED_BREP_SHAPE_REPRESENTATION('',(#416),#10261);
#354=ADVANCED_BREP_SHAPE_REPRESENTATION('',(#417),#10262);
#355=ADVANCED_BREP_SHAPE_REPRESENTATION('',(#418),#10263);
#356=ADVANCED_BREP_SHAPE_REPRESENTATION('',(#39),#10264);
#357=STYLED_ITEM('',(#10641),#389);
#358=STYLED_ITEM('',(#10641),#390);
#359=STYLED_ITEM('',(#10641),#391);
#360=STYLED_ITEM('',(#10634),#392);
#361=STYLED_ITEM('',(#10641),#393);
#362=STYLED_ITEM('',(#10648),#394);
#363=STYLED_ITEM('',(#10655),#395);
#364=STYLED_ITEM('',(#10634),#396);
#365=STYLED_ITEM('',(#10648),#397);
#366=STYLED_ITEM('',(#10641),#398);
#367=STYLED_ITEM('',(#10648),#399);
#368=STYLED_ITEM('',(#10641),#400);
#369=STYLED_ITEM('',(#10648),#401);
#370=STYLED_ITEM('',(#10662),#402);
#371=STYLED_ITEM('',(#10655),#403);
#372=STYLED_ITEM('',(#10655),#404);
#373=STYLED_ITEM('',(#10655),#405);
#374=STYLED_ITEM('',(#10655),#406);
#375=STYLED_ITEM('',(#10669),#407);
#376=STYLED_ITEM('',(#10648),#408);
#377=STYLED_ITEM('',(#10662),#38);
#378=STYLED_ITEM('',(#10634),#409);
#379=STYLED_ITEM('',(#10669),#410);
#380=STYLED_ITEM('',(#10662),#411);
#381=STYLED_ITEM('',(#10662),#412);
#382=STYLED_ITEM('',(#10641),#413);
#383=STYLED_ITEM('',(#10655),#414);
#384=STYLED_ITEM('',(#10648),#415);
#385=STYLED_ITEM('',(#10662),#416);
#386=STYLED_ITEM('',(#10655),#417);
#387=STYLED_ITEM('',(#10662),#418);
#388=STYLED_ITEM('',(#10662),#39);
#389=MANIFOLD_SOLID_BREP('Body1',#5045);
#390=MANIFOLD_SOLID_BREP('Body1',#5046);
#391=MANIFOLD_SOLID_BREP('Body1',#5047);
#392=MANIFOLD_SOLID_BREP('Body1',#5048);
#393=MANIFOLD_SOLID_BREP('Body1',#5049);
#394=MANIFOLD_SOLID_BREP('Body1',#5050);
#395=MANIFOLD_SOLID_BREP('Body1',#5051);
#396=MANIFOLD_SOLID_BREP('Body1',#5052);
#397=MANIFOLD_SOLID_BREP('Body1',#5053);
#398=MANIFOLD_SOLID_BREP('Body1',#5054);
#399=MANIFOLD_SOLID_BREP('Body1',#5055);
#400=MANIFOLD_SOLID_BREP('Body1',#5056);
#401=MANIFOLD_SOLID_BREP('Body1',#5057);
#402=MANIFOLD_SOLID_BREP('Body1',#5058);
#403=MANIFOLD_SOLID_BREP('Body1',#5059);
#404=MANIFOLD_SOLID_BREP('Body1',#5060);
#405=MANIFOLD_SOLID_BREP('Body1',#5061);
#406=MANIFOLD_SOLID_BREP('Body1',#5062);
#407=MANIFOLD_SOLID_BREP('Body1',#5063);
#408=MANIFOLD_SOLID_BREP('Body1',#5064);
#409=MANIFOLD_SOLID_BREP('Body1',#5067);
#410=MANIFOLD_SOLID_BREP('Body1',#5068);
#411=MANIFOLD_SOLID_BREP('Body1',#5069);
#412=MANIFOLD_SOLID_BREP('Body1',#5070);
#413=MANIFOLD_SOLID_BREP('Body1',#5071);
#414=MANIFOLD_SOLID_BREP('Body1',#5072);
#415=MANIFOLD_SOLID_BREP('Body1',#5073);
#416=MANIFOLD_SOLID_BREP('Body1',#5074);
#417=MANIFOLD_SOLID_BREP('Body1',#5075);
#418=MANIFOLD_SOLID_BREP('Body1',#5076);
#419=FACE_BOUND('',#1064,.T.);
#420=FACE_BOUND('',#1065,.T.);
#421=FACE_BOUND('',#1066,.T.);
#422=FACE_BOUND('',#1067,.T.);
#423=FACE_BOUND('',#1068,.T.);
#424=FACE_BOUND('',#1069,.T.);
#425=FACE_BOUND('',#1070,.T.);
#426=FACE_BOUND('',#1071,.T.);
#427=FACE_BOUND('',#1072,.T.);
#428=FACE_BOUND('',#1074,.T.);
#429=FACE_BOUND('',#1075,.T.);
#430=FACE_BOUND('',#1076,.T.);
#431=FACE_BOUND('',#1077,.T.);
#432=FACE_BOUND('',#1078,.T.);
#433=FACE_BOUND('',#1079,.T.);
#434=FACE_BOUND('',#1080,.T.);
#435=FACE_BOUND('',#1081,.T.);
#436=FACE_BOUND('',#1082,.T.);
#437=FACE_BOUND('',#1113,.T.);
#438=FACE_BOUND('',#1120,.T.);
#439=FACE_BOUND('',#1121,.T.);
#440=FACE_BOUND('',#1122,.T.);
#441=FACE_BOUND('',#1123,.T.);
#442=FACE_BOUND('',#1124,.T.);
#443=FACE_BOUND('',#1126,.T.);
#444=FACE_BOUND('',#1127,.T.);
#445=FACE_BOUND('',#1128,.T.);
#446=FACE_BOUND('',#1129,.T.);
#447=FACE_BOUND('',#1130,.T.);
#448=FACE_BOUND('',#1133,.T.);
#449=FACE_BOUND('',#1136,.T.);
#450=FACE_BOUND('',#1139,.T.);
#451=FACE_BOUND('',#1142,.T.);
#452=FACE_BOUND('',#1149,.T.);
#453=FACE_BOUND('',#1153,.T.);
#454=FACE_BOUND('',#1154,.T.);
#455=FACE_BOUND('',#1155,.T.);
#456=FACE_BOUND('',#1156,.T.);
#457=FACE_BOUND('',#1157,.T.);
#458=FACE_BOUND('',#1159,.T.);
#459=FACE_BOUND('',#1160,.T.);
#460=FACE_BOUND('',#1161,.T.);
#461=FACE_BOUND('',#1162,.T.);
#462=FACE_BOUND('',#1163,.T.);
#463=FACE_BOUND('',#1167,.T.);
#464=FACE_BOUND('',#1169,.T.);
#465=FACE_BOUND('',#1184,.T.);
#466=FACE_BOUND('',#1191,.T.);
#467=FACE_BOUND('',#1194,.T.);
#468=FACE_BOUND('',#1198,.T.);
#469=FACE_BOUND('',#1205,.T.);
#470=FACE_BOUND('',#1206,.T.);
#471=FACE_BOUND('',#1207,.T.);
#472=FACE_BOUND('',#1208,.T.);
#473=FACE_BOUND('',#1209,.T.);
#474=FACE_BOUND('',#1211,.T.);
#475=FACE_BOUND('',#1212,.T.);
#476=FACE_BOUND('',#1213,.T.);
#477=FACE_BOUND('',#1214,.T.);
#478=FACE_BOUND('',#1218,.T.);
#479=FACE_BOUND('',#1220,.T.);
#480=FACE_BOUND('',#1227,.T.);
#481=FACE_BOUND('',#1230,.T.);
#482=FACE_BOUND('',#1233,.T.);
#483=FACE_BOUND('',#1235,.T.);
#484=FACE_BOUND('',#1240,.T.);
#485=FACE_BOUND('',#1243,.T.);
#486=FACE_BOUND('',#1244,.T.);
#487=FACE_BOUND('',#1250,.T.);
#488=FACE_BOUND('',#1252,.T.);
#489=FACE_BOUND('',#1253,.T.);
#490=FACE_BOUND('',#1254,.T.);
#491=FACE_BOUND('',#1255,.T.);
#492=FACE_BOUND('',#1256,.T.);
#493=FACE_BOUND('',#1258,.T.);
#494=FACE_BOUND('',#1259,.T.);
#495=FACE_BOUND('',#1260,.T.);
#496=FACE_BOUND('',#1261,.T.);
#497=FACE_BOUND('',#1262,.T.);
#498=FACE_BOUND('',#1266,.T.);
#499=FACE_BOUND('',#1268,.T.);
#500=FACE_BOUND('',#1272,.T.);
#501=FACE_BOUND('',#1274,.T.);
#502=FACE_BOUND('',#1278,.T.);
#503=FACE_BOUND('',#1280,.T.);
#504=FACE_BOUND('',#1299,.T.);
#505=FACE_BOUND('',#1302,.T.);
#506=FACE_BOUND('',#1305,.T.);
#507=FACE_BOUND('',#1308,.T.);
#508=FACE_BOUND('',#1311,.T.);
#509=FACE_BOUND('',#1314,.T.);
#510=FACE_BOUND('',#1316,.T.);
#511=FACE_BOUND('',#1322,.T.);
#512=FACE_BOUND('',#1324,.T.);
#513=FACE_BOUND('',#1326,.T.);
#514=FACE_BOUND('',#1328,.T.);
#515=FACE_BOUND('',#1334,.T.);
#516=FACE_BOUND('',#1349,.T.);
#517=FACE_BOUND('',#1351,.T.);
#518=FACE_BOUND('',#1353,.T.);
#519=FACE_BOUND('',#1361,.T.);
#520=FACE_BOUND('',#1364,.T.);
#521=FACE_BOUND('',#1368,.T.);
#522=FACE_BOUND('',#1371,.T.);
#523=FACE_BOUND('',#1374,.T.);
#524=FACE_BOUND('',#1377,.T.);
#525=FACE_BOUND('',#1382,.T.);
#526=FACE_BOUND('',#1385,.T.);
#527=FACE_BOUND('',#1396,.T.);
#528=FACE_BOUND('',#1398,.T.);
#529=FACE_BOUND('',#1401,.T.);
#530=FACE_BOUND('',#1408,.T.);
#531=FACE_BOUND('',#1416,.T.);
#532=FACE_BOUND('',#1421,.T.);
#533=FACE_BOUND('',#1423,.T.);
#534=FACE_BOUND('',#1426,.T.);
#535=FACE_BOUND('',#1435,.T.);
#536=FACE_BOUND('',#1437,.T.);
#537=FACE_BOUND('',#1440,.T.);
#538=FACE_BOUND('',#1442,.T.);
#539=FACE_BOUND('',#1447,.T.);
#540=FACE_BOUND('',#1449,.T.);
#541=FACE_BOUND('',#1453,.T.);
#542=FACE_BOUND('',#1455,.T.);
#543=FACE_BOUND('',#1469,.T.);
#544=FACE_BOUND('',#1477,.T.);
#545=PLANE('',#5462);
#546=PLANE('',#5463);
#547=PLANE('',#5464);
#548=PLANE('',#5465);
#549=PLANE('',#5466);
#550=PLANE('',#5467);
#551=PLANE('',#5469);
#552=PLANE('',#5470);
#553=PLANE('',#5471);
#554=PLANE('',#5472);
#555=PLANE('',#5473);
#556=PLANE('',#5474);
#557=PLANE('',#5476);
#558=PLANE('',#5477);
#559=PLANE('',#5478);
#560=PLANE('',#5479);
#561=PLANE('',#5480);
#562=PLANE('',#5481);
#563=PLANE('',#5486);
#564=PLANE('',#5490);
#565=PLANE('',#5494);
#566=PLANE('',#5498);
#567=PLANE('',#5502);
#568=PLANE('',#5506);
#569=PLANE('',#5510);
#570=PLANE('',#5514);
#571=PLANE('',#5518);
#572=PLANE('',#5522);
#573=PLANE('',#5523);
#574=PLANE('',#5524);
#575=PLANE('',#5525);
#576=PLANE('',#5526);
#577=PLANE('',#5527);
#578=PLANE('',#5532);
#579=PLANE('',#5537);
#580=PLANE('',#5542);
#581=PLANE('',#5547);
#582=PLANE('',#5560);
#583=PLANE('',#5567);
#584=PLANE('',#5568);
#585=PLANE('',#5576);
#586=PLANE('',#5577);
#587=PLANE('',#5581);
#588=PLANE('',#5582);
#589=PLANE('',#5587);
#590=PLANE('',#5588);
#591=PLANE('',#5589);
#592=PLANE('',#5590);
#593=PLANE('',#5591);
#594=PLANE('',#5592);
#595=PLANE('',#5593);
#596=PLANE('',#5594);
#597=PLANE('',#5595);
#598=PLANE('',#5596);
#599=PLANE('',#5600);
#600=PLANE('',#5604);
#601=PLANE('',#5610);
#602=PLANE('',#5613);
#603=PLANE('',#5621);
#604=PLANE('',#5636);
#605=PLANE('',#5637);
#606=PLANE('',#5645);
#607=PLANE('',#5646);
#608=PLANE('',#5648);
#609=PLANE('',#5652);
#610=PLANE('',#5660);
#611=PLANE('',#5663);
#612=PLANE('',#5667);
#613=PLANE('',#5669);
#614=PLANE('',#5678);
#615=PLANE('',#5682);
#616=PLANE('',#5698);
#617=PLANE('',#5699);
#618=PLANE('',#5707);
#619=PLANE('',#5708);
#620=PLANE('',#5716);
#621=PLANE('',#5717);
#622=PLANE('',#5725);
#623=PLANE('',#5726);
#624=PLANE('',#5731);
#625=PLANE('',#5732);
#626=PLANE('',#5737);
#627=PLANE('',#5738);
#628=PLANE('',#5743);
#629=PLANE('',#5744);
#630=PLANE('',#5749);
#631=PLANE('',#5750);
#632=PLANE('',#5753);
#633=PLANE('',#5755);
#634=PLANE('',#5756);
#635=PLANE('',#5758);
#636=PLANE('',#5759);
#637=PLANE('',#5760);
#638=PLANE('',#5765);
#639=PLANE('',#5769);
#640=PLANE('',#5773);
#641=PLANE('',#5777);
#642=PLANE('',#5781);
#643=PLANE('',#5785);
#644=PLANE('',#5788);
#645=PLANE('',#5789);
#646=PLANE('',#5792);
#647=PLANE('',#5793);
#648=PLANE('',#5798);
#649=PLANE('',#5804);
#650=PLANE('',#5812);
#651=PLANE('',#5820);
#652=PLANE('',#5821);
#653=PLANE('',#5822);
#654=PLANE('',#5823);
#655=PLANE('',#5824);
#656=PLANE('',#5825);
#657=PLANE('',#5826);
#658=PLANE('',#5827);
#659=PLANE('',#5828);
#660=PLANE('',#5834);
#661=PLANE('',#5836);
#662=PLANE('',#5838);
#663=PLANE('',#5840);
#664=PLANE('',#5841);
#665=PLANE('',#5842);
#666=PLANE('',#5843);
#667=PLANE('',#5844);
#668=PLANE('',#5845);
#669=PLANE('',#5846);
#670=PLANE('',#5850);
#671=PLANE('',#5855);
#672=PLANE('',#5859);
#673=PLANE('',#5864);
#674=PLANE('',#5868);
#675=PLANE('',#5879);
#676=PLANE('',#5883);
#677=PLANE('',#5889);
#678=PLANE('',#5890);
#679=PLANE('',#5891);
#680=PLANE('',#5895);
#681=PLANE('',#5896);
#682=PLANE('',#5897);
#683=PLANE('',#5898);
#684=PLANE('',#5899);
#685=PLANE('',#5905);
#686=PLANE('',#5909);
#687=PLANE('',#5910);
#688=PLANE('',#5911);
#689=PLANE('',#5912);
#690=PLANE('',#5913);
#691=PLANE('',#5914);
#692=PLANE('',#5915);
#693=PLANE('',#5916);
#694=PLANE('',#5920);
#695=PLANE('',#5921);
#696=PLANE('',#5929);
#697=PLANE('',#5930);
#698=PLANE('',#5932);
#699=PLANE('',#5939);
#700=PLANE('',#5940);
#701=PLANE('',#5941);
#702=PLANE('',#5942);
#703=PLANE('',#5943);
#704=PLANE('',#5948);
#705=PLANE('',#5952);
#706=PLANE('',#5956);
#707=PLANE('',#5957);
#708=PLANE('',#5962);
#709=PLANE('',#5964);
#710=PLANE('',#5973);
#711=PLANE('',#5974);
#712=PLANE('',#5982);
#713=PLANE('',#5983);
#714=PLANE('',#5985);
#715=PLANE('',#5991);
#716=PLANE('',#5993);
#717=PLANE('',#5995);
#718=PLANE('',#5996);
#719=PLANE('',#5997);
#720=PLANE('',#5998);
#721=PLANE('',#5999);
#722=PLANE('',#6000);
#723=PLANE('',#6001);
#724=PLANE('',#6002);
#725=PLANE('',#6008);
#726=PLANE('',#6016);
#727=PLANE('',#6024);
#728=PLANE('',#6025);
#729=PLANE('',#6026);
#730=PLANE('',#6027);
#731=PLANE('',#6028);
#732=PLANE('',#6029);
#733=PLANE('',#6030);
#734=PLANE('',#6031);
#735=PLANE('',#6032);
#736=FACE_OUTER_BOUND('',#1050,.T.);
#737=FACE_OUTER_BOUND('',#1051,.T.);
#738=FACE_OUTER_BOUND('',#1052,.T.);
#739=FACE_OUTER_BOUND('',#1053,.T.);
#740=FACE_OUTER_BOUND('',#1054,.T.);
#741=FACE_OUTER_BOUND('',#1055,.T.);
#742=FACE_OUTER_BOUND('',#1056,.T.);
#743=FACE_OUTER_BOUND('',#1057,.T.);
#744=FACE_OUTER_BOUND('',#1058,.T.);
#745=FACE_OUTER_BOUND('',#1059,.T.);
#746=FACE_OUTER_BOUND('',#1060,.T.);
#747=FACE_OUTER_BOUND('',#1061,.T.);
#748=FACE_OUTER_BOUND('',#1062,.T.);
#749=FACE_OUTER_BOUND('',#1063,.T.);
#750=FACE_OUTER_BOUND('',#1073,.T.);
#751=FACE_OUTER_BOUND('',#1083,.T.);
#752=FACE_OUTER_BOUND('',#1084,.T.);
#753=FACE_OUTER_BOUND('',#1085,.T.);
#754=FACE_OUTER_BOUND('',#1086,.T.);
#755=FACE_OUTER_BOUND('',#1087,.T.);
#756=FACE_OUTER_BOUND('',#1088,.T.);
#757=FACE_OUTER_BOUND('',#1089,.T.);
#758=FACE_OUTER_BOUND('',#1090,.T.);
#759=FACE_OUTER_BOUND('',#1091,.T.);
#760=FACE_OUTER_BOUND('',#1092,.T.);
#761=FACE_OUTER_BOUND('',#1093,.T.);
#762=FACE_OUTER_BOUND('',#1094,.T.);
#763=FACE_OUTER_BOUND('',#1095,.T.);
#764=FACE_OUTER_BOUND('',#1096,.T.);
#765=FACE_OUTER_BOUND('',#1097,.T.);
#766=FACE_OUTER_BOUND('',#1098,.T.);
#767=FACE_OUTER_BOUND('',#1099,.T.);
#768=FACE_OUTER_BOUND('',#1100,.T.);
#769=FACE_OUTER_BOUND('',#1101,.T.);
#770=FACE_OUTER_BOUND('',#1102,.T.);
#771=FACE_OUTER_BOUND('',#1103,.T.);
#772=FACE_OUTER_BOUND('',#1104,.T.);
#773=FACE_OUTER_BOUND('',#1105,.T.);
#774=FACE_OUTER_BOUND('',#1106,.T.);
#775=FACE_OUTER_BOUND('',#1107,.T.);
#776=FACE_OUTER_BOUND('',#1108,.T.);
#777=FACE_OUTER_BOUND('',#1109,.T.);
#778=FACE_OUTER_BOUND('',#1110,.T.);
#779=FACE_OUTER_BOUND('',#1111,.T.);
#780=FACE_OUTER_BOUND('',#1112,.T.);
#781=FACE_OUTER_BOUND('',#1114,.T.);
#782=FACE_OUTER_BOUND('',#1115,.T.);
#783=FACE_OUTER_BOUND('',#1116,.T.);
#784=FACE_OUTER_BOUND('',#1117,.T.);
#785=FACE_OUTER_BOUND('',#1118,.T.);
#786=FACE_OUTER_BOUND('',#1119,.T.);
#787=FACE_OUTER_BOUND('',#1125,.T.);
#788=FACE_OUTER_BOUND('',#1131,.T.);
#789=FACE_OUTER_BOUND('',#1132,.T.);
#790=FACE_OUTER_BOUND('',#1134,.T.);
#791=FACE_OUTER_BOUND('',#1135,.T.);
#792=FACE_OUTER_BOUND('',#1137,.T.);
#793=FACE_OUTER_BOUND('',#1138,.T.);
#794=FACE_OUTER_BOUND('',#1140,.T.);
#795=FACE_OUTER_BOUND('',#1141,.T.);
#796=FACE_OUTER_BOUND('',#1143,.T.);
#797=FACE_OUTER_BOUND('',#1144,.T.);
#798=FACE_OUTER_BOUND('',#1145,.T.);
#799=FACE_OUTER_BOUND('',#1146,.T.);
#800=FACE_OUTER_BOUND('',#1147,.T.);
#801=FACE_OUTER_BOUND('',#1148,.T.);
#802=FACE_OUTER_BOUND('',#1150,.T.);
#803=FACE_OUTER_BOUND('',#1151,.T.);
#804=FACE_OUTER_BOUND('',#1152,.T.);
#805=FACE_OUTER_BOUND('',#1158,.T.);
#806=FACE_OUTER_BOUND('',#1164,.T.);
#807=FACE_OUTER_BOUND('',#1165,.T.);
#808=FACE_OUTER_BOUND('',#1166,.T.);
#809=FACE_OUTER_BOUND('',#1168,.T.);
#810=FACE_OUTER_BOUND('',#1170,.T.);
#811=FACE_OUTER_BOUND('',#1171,.T.);
#812=FACE_OUTER_BOUND('',#1172,.T.);
#813=FACE_OUTER_BOUND('',#1173,.T.);
#814=FACE_OUTER_BOUND('',#1174,.T.);
#815=FACE_OUTER_BOUND('',#1175,.T.);
#816=FACE_OUTER_BOUND('',#1176,.T.);
#817=FACE_OUTER_BOUND('',#1177,.T.);
#818=FACE_OUTER_BOUND('',#1178,.T.);
#819=FACE_OUTER_BOUND('',#1179,.T.);
#820=FACE_OUTER_BOUND('',#1180,.T.);
#821=FACE_OUTER_BOUND('',#1181,.T.);
#822=FACE_OUTER_BOUND('',#1182,.T.);
#823=FACE_OUTER_BOUND('',#1183,.T.);
#824=FACE_OUTER_BOUND('',#1185,.T.);
#825=FACE_OUTER_BOUND('',#1186,.T.);
#826=FACE_OUTER_BOUND('',#1187,.T.);
#827=FACE_OUTER_BOUND('',#1188,.T.);
#828=FACE_OUTER_BOUND('',#1189,.T.);
#829=FACE_OUTER_BOUND('',#1190,.T.);
#830=FACE_OUTER_BOUND('',#1192,.T.);
#831=FACE_OUTER_BOUND('',#1193,.T.);
#832=FACE_OUTER_BOUND('',#1195,.T.);
#833=FACE_OUTER_BOUND('',#1196,.T.);
#834=FACE_OUTER_BOUND('',#1197,.T.);
#835=FACE_OUTER_BOUND('',#1199,.T.);
#836=FACE_OUTER_BOUND('',#1200,.T.);
#837=FACE_OUTER_BOUND('',#1201,.T.);
#838=FACE_OUTER_BOUND('',#1202,.T.);
#839=FACE_OUTER_BOUND('',#1203,.T.);
#840=FACE_OUTER_BOUND('',#1204,.T.);
#841=FACE_OUTER_BOUND('',#1210,.T.);
#842=FACE_OUTER_BOUND('',#1215,.T.);
#843=FACE_OUTER_BOUND('',#1216,.T.);
#844=FACE_OUTER_BOUND('',#1217,.T.);
#845=FACE_OUTER_BOUND('',#1219,.T.);
#846=FACE_OUTER_BOUND('',#1221,.T.);
#847=FACE_OUTER_BOUND('',#1222,.T.);
#848=FACE_OUTER_BOUND('',#1223,.T.);
#849=FACE_OUTER_BOUND('',#1224,.T.);
#850=FACE_OUTER_BOUND('',#1225,.T.);
#851=FACE_OUTER_BOUND('',#1226,.T.);
#852=FACE_OUTER_BOUND('',#1228,.T.);
#853=FACE_OUTER_BOUND('',#1229,.T.);
#854=FACE_OUTER_BOUND('',#1231,.T.);
#855=FACE_OUTER_BOUND('',#1232,.T.);
#856=FACE_OUTER_BOUND('',#1234,.T.);
#857=FACE_OUTER_BOUND('',#1236,.T.);
#858=FACE_OUTER_BOUND('',#1237,.T.);
#859=FACE_OUTER_BOUND('',#1238,.T.);
#860=FACE_OUTER_BOUND('',#1239,.T.);
#861=FACE_OUTER_BOUND('',#1241,.T.);
#862=FACE_OUTER_BOUND('',#1242,.T.);
#863=FACE_OUTER_BOUND('',#1245,.T.);
#864=FACE_OUTER_BOUND('',#1246,.T.);
#865=FACE_OUTER_BOUND('',#1247,.T.);
#866=FACE_OUTER_BOUND('',#1248,.T.);
#867=FACE_OUTER_BOUND('',#1249,.T.);
#868=FACE_OUTER_BOUND('',#1251,.T.);
#869=FACE_OUTER_BOUND('',#1257,.T.);
#870=FACE_OUTER_BOUND('',#1263,.T.);
#871=FACE_OUTER_BOUND('',#1264,.T.);
#872=FACE_OUTER_BOUND('',#1265,.T.);
#873=FACE_OUTER_BOUND('',#1267,.T.);
#874=FACE_OUTER_BOUND('',#1269,.T.);
#875=FACE_OUTER_BOUND('',#1270,.T.);
#876=FACE_OUTER_BOUND('',#1271,.T.);
#877=FACE_OUTER_BOUND('',#1273,.T.);
#878=FACE_OUTER_BOUND('',#1275,.T.);
#879=FACE_OUTER_BOUND('',#1276,.T.);
#880=FACE_OUTER_BOUND('',#1277,.T.);
#881=FACE_OUTER_BOUND('',#1279,.T.);
#882=FACE_OUTER_BOUND('',#1281,.T.);
#883=FACE_OUTER_BOUND('',#1282,.T.);
#884=FACE_OUTER_BOUND('',#1283,.T.);
#885=FACE_OUTER_BOUND('',#1284,.T.);
#886=FACE_OUTER_BOUND('',#1285,.T.);
#887=FACE_OUTER_BOUND('',#1286,.T.);
#888=FACE_OUTER_BOUND('',#1287,.T.);
#889=FACE_OUTER_BOUND('',#1288,.T.);
#890=FACE_OUTER_BOUND('',#1289,.T.);
#891=FACE_OUTER_BOUND('',#1290,.T.);
#892=FACE_OUTER_BOUND('',#1291,.T.);
#893=FACE_OUTER_BOUND('',#1292,.T.);
#894=FACE_OUTER_BOUND('',#1293,.T.);
#895=FACE_OUTER_BOUND('',#1294,.T.);
#896=FACE_OUTER_BOUND('',#1295,.T.);
#897=FACE_OUTER_BOUND('',#1296,.T.);
#898=FACE_OUTER_BOUND('',#1297,.T.);
#899=FACE_OUTER_BOUND('',#1298,.T.);
#900=FACE_OUTER_BOUND('',#1300,.T.);
#901=FACE_OUTER_BOUND('',#1301,.T.);
#902=FACE_OUTER_BOUND('',#1303,.T.);
#903=FACE_OUTER_BOUND('',#1304,.T.);
#904=FACE_OUTER_BOUND('',#1306,.T.);
#905=FACE_OUTER_BOUND('',#1307,.T.);
#906=FACE_OUTER_BOUND('',#1309,.T.);
#907=FACE_OUTER_BOUND('',#1310,.T.);
#908=FACE_OUTER_BOUND('',#1312,.T.);
#909=FACE_OUTER_BOUND('',#1313,.T.);
#910=FACE_OUTER_BOUND('',#1315,.T.);
#911=FACE_OUTER_BOUND('',#1317,.T.);
#912=FACE_OUTER_BOUND('',#1318,.T.);
#913=FACE_OUTER_BOUND('',#1319,.T.);
#914=FACE_OUTER_BOUND('',#1320,.T.);
#915=FACE_OUTER_BOUND('',#1321,.T.);
#916=FACE_OUTER_BOUND('',#1323,.T.);
#917=FACE_OUTER_BOUND('',#1325,.T.);
#918=FACE_OUTER_BOUND('',#1327,.T.);
#919=FACE_OUTER_BOUND('',#1329,.T.);
#920=FACE_OUTER_BOUND('',#1330,.T.);
#921=FACE_OUTER_BOUND('',#1331,.T.);
#922=FACE_OUTER_BOUND('',#1332,.T.);
#923=FACE_OUTER_BOUND('',#1333,.T.);
#924=FACE_OUTER_BOUND('',#1335,.T.);
#925=FACE_OUTER_BOUND('',#1336,.T.);
#926=FACE_OUTER_BOUND('',#1337,.T.);
#927=FACE_OUTER_BOUND('',#1338,.T.);
#928=FACE_OUTER_BOUND('',#1339,.T.);
#929=FACE_OUTER_BOUND('',#1340,.T.);
#930=FACE_OUTER_BOUND('',#1341,.T.);
#931=FACE_OUTER_BOUND('',#1342,.T.);
#932=FACE_OUTER_BOUND('',#1343,.T.);
#933=FACE_OUTER_BOUND('',#1344,.T.);
#934=FACE_OUTER_BOUND('',#1345,.T.);
#935=FACE_OUTER_BOUND('',#1346,.T.);
#936=FACE_OUTER_BOUND('',#1347,.T.);
#937=FACE_OUTER_BOUND('',#1348,.T.);
#938=FACE_OUTER_BOUND('',#1350,.T.);
#939=FACE_OUTER_BOUND('',#1352,.T.);
#940=FACE_OUTER_BOUND('',#1354,.T.);
#941=FACE_OUTER_BOUND('',#1355,.T.);
#942=FACE_OUTER_BOUND('',#1356,.T.);
#943=FACE_OUTER_BOUND('',#1357,.T.);
#944=FACE_OUTER_BOUND('',#1358,.T.);
#945=FACE_OUTER_BOUND('',#1359,.T.);
#946=FACE_OUTER_BOUND('',#1360,.T.);
#947=FACE_OUTER_BOUND('',#1362,.T.);
#948=FACE_OUTER_BOUND('',#1363,.T.);
#949=FACE_OUTER_BOUND('',#1365,.T.);
#950=FACE_OUTER_BOUND('',#1366,.T.);
#951=FACE_OUTER_BOUND('',#1367,.T.);
#952=FACE_OUTER_BOUND('',#1369,.T.);
#953=FACE_OUTER_BOUND('',#1370,.T.);
#954=FACE_OUTER_BOUND('',#1372,.T.);
#955=FACE_OUTER_BOUND('',#1373,.T.);
#956=FACE_OUTER_BOUND('',#1375,.T.);
#957=FACE_OUTER_BOUND('',#1376,.T.);
#958=FACE_OUTER_BOUND('',#1378,.T.);
#959=FACE_OUTER_BOUND('',#1379,.T.);
#960=FACE_OUTER_BOUND('',#1380,.T.);
#961=FACE_OUTER_BOUND('',#1381,.T.);
#962=FACE_OUTER_BOUND('',#1383,.T.);
#963=FACE_OUTER_BOUND('',#1384,.T.);
#964=FACE_OUTER_BOUND('',#1386,.T.);
#965=FACE_OUTER_BOUND('',#1387,.T.);
#966=FACE_OUTER_BOUND('',#1388,.T.);
#967=FACE_OUTER_BOUND('',#1389,.T.);
#968=FACE_OUTER_BOUND('',#1390,.T.);
#969=FACE_OUTER_BOUND('',#1391,.T.);
#970=FACE_OUTER_BOUND('',#1392,.T.);
#971=FACE_OUTER_BOUND('',#1393,.T.);
#972=FACE_OUTER_BOUND('',#1394,.T.);
#973=FACE_OUTER_BOUND('',#1395,.T.);
#974=FACE_OUTER_BOUND('',#1397,.T.);
#975=FACE_OUTER_BOUND('',#1399,.T.);
#976=FACE_OUTER_BOUND('',#1400,.T.);
#977=FACE_OUTER_BOUND('',#1402,.T.);
#978=FACE_OUTER_BOUND('',#1403,.T.);
#979=FACE_OUTER_BOUND('',#1404,.T.);
#980=FACE_OUTER_BOUND('',#1405,.T.);
#981=FACE_OUTER_BOUND('',#1406,.T.);
#982=FACE_OUTER_BOUND('',#1407,.T.);
#983=FACE_OUTER_BOUND('',#1409,.T.);
#984=FACE_OUTER_BOUND('',#1410,.T.);
#985=FACE_OUTER_BOUND('',#1411,.T.);
#986=FACE_OUTER_BOUND('',#1412,.T.);
#987=FACE_OUTER_BOUND('',#1413,.T.);
#988=FACE_OUTER_BOUND('',#1414,.T.);
#989=FACE_OUTER_BOUND('',#1415,.T.);
#990=FACE_OUTER_BOUND('',#1417,.T.);
#991=FACE_OUTER_BOUND('',#1418,.T.);
#992=FACE_OUTER_BOUND('',#1419,.T.);
#993=FACE_OUTER_BOUND('',#1420,.T.);
#994=FACE_OUTER_BOUND('',#1422,.T.);
#995=FACE_OUTER_BOUND('',#1424,.T.);
#996=FACE_OUTER_BOUND('',#1425,.T.);
#997=FACE_OUTER_BOUND('',#1427,.T.);
#998=FACE_OUTER_BOUND('',#1428,.T.);
#999=FACE_OUTER_BOUND('',#1429,.T.);
#1000=FACE_OUTER_BOUND('',#1430,.T.);
#1001=FACE_OUTER_BOUND('',#1431,.T.);
#1002=FACE_OUTER_BOUND('',#1432,.T.);
#1003=FACE_OUTER_BOUND('',#1433,.T.);
#1004=FACE_OUTER_BOUND('',#1434,.T.);
#1005=FACE_OUTER_BOUND('',#1436,.T.);
#1006=FACE_OUTER_BOUND('',#1438,.T.);
#1007=FACE_OUTER_BOUND('',#1439,.T.);
#1008=FACE_OUTER_BOUND('',#1441,.T.);
#1009=FACE_OUTER_BOUND('',#1443,.T.);
#1010=FACE_OUTER_BOUND('',#1444,.T.);
#1011=FACE_OUTER_BOUND('',#1445,.T.);
#1012=FACE_OUTER_BOUND('',#1446,.T.);
#1013=FACE_OUTER_BOUND('',#1448,.T.);
#1014=FACE_OUTER_BOUND('',#1450,.T.);
#1015=FACE_OUTER_BOUND('',#1451,.T.);
#1016=FACE_OUTER_BOUND('',#1452,.T.);
#1017=FACE_OUTER_BOUND('',#1454,.T.);
#1018=FACE_OUTER_BOUND('',#1456,.T.);
#1019=FACE_OUTER_BOUND('',#1457,.T.);
#1020=FACE_OUTER_BOUND('',#1458,.T.);
#1021=FACE_OUTER_BOUND('',#1459,.T.);
#1022=FACE_OUTER_BOUND('',#1460,.T.);
#1023=FACE_OUTER_BOUND('',#1461,.T.);
#1024=FACE_OUTER_BOUND('',#1462,.T.);
#1025=FACE_OUTER_BOUND('',#1463,.T.);
#1026=FACE_OUTER_BOUND('',#1464,.T.);
#1027=FACE_OUTER_BOUND('',#1465,.T.);
#1028=FACE_OUTER_BOUND('',#1466,.T.);
#1029=FACE_OUTER_BOUND('',#1467,.T.);
#1030=FACE_OUTER_BOUND('',#1468,.T.);
#1031=FACE_OUTER_BOUND('',#1470,.T.);
#1032=FACE_OUTER_BOUND('',#1471,.T.);
#1033=FACE_OUTER_BOUND('',#1472,.T.);
#1034=FACE_OUTER_BOUND('',#1473,.T.);
#1035=FACE_OUTER_BOUND('',#1474,.T.);
#1036=FACE_OUTER_BOUND('',#1475,.T.);
#1037=FACE_OUTER_BOUND('',#1476,.T.);
#1038=FACE_OUTER_BOUND('',#1478,.T.);
#1039=FACE_OUTER_BOUND('',#1479,.T.);
#1040=FACE_OUTER_BOUND('',#1480,.T.);
#1041=FACE_OUTER_BOUND('',#1481,.T.);
#1042=FACE_OUTER_BOUND('',#1482,.T.);
#1043=FACE_OUTER_BOUND('',#1483,.T.);
#1044=FACE_OUTER_BOUND('',#1484,.T.);
#1045=FACE_OUTER_BOUND('',#1485,.T.);
#1046=FACE_OUTER_BOUND('',#1486,.T.);
#1047=FACE_OUTER_BOUND('',#1487,.T.);
#1048=FACE_OUTER_BOUND('',#1488,.T.);
#1049=FACE_OUTER_BOUND('',#1489,.T.);
#1050=EDGE_LOOP('',(#3410,#3411,#3412,#3413));
#1051=EDGE_LOOP('',(#3414,#3415,#3416,#3417));
#1052=EDGE_LOOP('',(#3418,#3419,#3420,#3421));
#1053=EDGE_LOOP('',(#3422,#3423,#3424,#3425));
#1054=EDGE_LOOP('',(#3426,#3427,#3428,#3429));
#1055=EDGE_LOOP('',(#3430,#3431,#3432,#3433));
#1056=EDGE_LOOP('',(#3434,#3435,#3436,#3437));
#1057=EDGE_LOOP('',(#3438,#3439,#3440,#3441));
#1058=EDGE_LOOP('',(#3442,#3443,#3444,#3445));
#1059=EDGE_LOOP('',(#3446,#3447,#3448,#3449));
#1060=EDGE_LOOP('',(#3450,#3451,#3452,#3453));
#1061=EDGE_LOOP('',(#3454,#3455,#3456,#3457));
#1062=EDGE_LOOP('',(#3458,#3459,#3460,#3461));
#1063=EDGE_LOOP('',(#3462,#3463,#3464,#3465));
#1064=EDGE_LOOP('',(#3466));
#1065=EDGE_LOOP('',(#3467));
#1066=EDGE_LOOP('',(#3468));
#1067=EDGE_LOOP('',(#3469));
#1068=EDGE_LOOP('',(#3470));
#1069=EDGE_LOOP('',(#3471));
#1070=EDGE_LOOP('',(#3472));
#1071=EDGE_LOOP('',(#3473));
#1072=EDGE_LOOP('',(#3474));
#1073=EDGE_LOOP('',(#3475,#3476,#3477,#3478));
#1074=EDGE_LOOP('',(#3479));
#1075=EDGE_LOOP('',(#3480));
#1076=EDGE_LOOP('',(#3481));
#1077=EDGE_LOOP('',(#3482));
#1078=EDGE_LOOP('',(#3483));
#1079=EDGE_LOOP('',(#3484));
#1080=EDGE_LOOP('',(#3485));
#1081=EDGE_LOOP('',(#3486));
#1082=EDGE_LOOP('',(#3487));
#1083=EDGE_LOOP('',(#3488,#3489,#3490,#3491));
#1084=EDGE_LOOP('',(#3492,#3493,#3494,#3495));
#1085=EDGE_LOOP('',(#3496,#3497,#3498,#3499));
#1086=EDGE_LOOP('',(#3500,#3501,#3502,#3503));
#1087=EDGE_LOOP('',(#3504,#3505,#3506,#3507));
#1088=EDGE_LOOP('',(#3508,#3509,#3510,#3511));
#1089=EDGE_LOOP('',(#3512,#3513,#3514,#3515));
#1090=EDGE_LOOP('',(#3516,#3517,#3518,#3519));
#1091=EDGE_LOOP('',(#3520,#3521,#3522,#3523));
#1092=EDGE_LOOP('',(#3524,#3525,#3526,#3527));
#1093=EDGE_LOOP('',(#3528,#3529,#3530,#3531));
#1094=EDGE_LOOP('',(#3532,#3533,#3534,#3535));
#1095=EDGE_LOOP('',(#3536,#3537,#3538,#3539));
#1096=EDGE_LOOP('',(#3540));
#1097=EDGE_LOOP('',(#3541,#3542,#3543,#3544));
#1098=EDGE_LOOP('',(#3545));
#1099=EDGE_LOOP('',(#3546,#3547,#3548,#3549));
#1100=EDGE_LOOP('',(#3550));
#1101=EDGE_LOOP('',(#3551,#3552,#3553,#3554));
#1102=EDGE_LOOP('',(#3555));
#1103=EDGE_LOOP('',(#3556,#3557,#3558,#3559));
#1104=EDGE_LOOP('',(#3560));
#1105=EDGE_LOOP('',(#3561,#3562,#3563,#3564));
#1106=EDGE_LOOP('',(#3565));
#1107=EDGE_LOOP('',(#3566,#3567,#3568,#3569));
#1108=EDGE_LOOP('',(#3570));
#1109=EDGE_LOOP('',(#3571,#3572,#3573,#3574));
#1110=EDGE_LOOP('',(#3575));
#1111=EDGE_LOOP('',(#3576,#3577,#3578,#3579));
#1112=EDGE_LOOP('',(#3580));
#1113=EDGE_LOOP('',(#3581));
#1114=EDGE_LOOP('',(#3582,#3583,#3584,#3585));
#1115=EDGE_LOOP('',(#3586,#3587,#3588,#3589));
#1116=EDGE_LOOP('',(#3590,#3591,#3592,#3593));
#1117=EDGE_LOOP('',(#3594,#3595,#3596,#3597));
#1118=EDGE_LOOP('',(#3598,#3599,#3600,#3601));
#1119=EDGE_LOOP('',(#3602,#3603,#3604,#3605));
#1120=EDGE_LOOP('',(#3606));
#1121=EDGE_LOOP('',(#3607));
#1122=EDGE_LOOP('',(#3608));
#1123=EDGE_LOOP('',(#3609));
#1124=EDGE_LOOP('',(#3610));
#1125=EDGE_LOOP('',(#3611,#3612,#3613,#3614));
#1126=EDGE_LOOP('',(#3615));
#1127=EDGE_LOOP('',(#3616));
#1128=EDGE_LOOP('',(#3617));
#1129=EDGE_LOOP('',(#3618));
#1130=EDGE_LOOP('',(#3619));
#1131=EDGE_LOOP('',(#3620,#3621,#3622,#3623));
#1132=EDGE_LOOP('',(#3624));
#1133=EDGE_LOOP('',(#3625));
#1134=EDGE_LOOP('',(#3626,#3627,#3628,#3629));
#1135=EDGE_LOOP('',(#3630));
#1136=EDGE_LOOP('',(#3631));
#1137=EDGE_LOOP('',(#3632,#3633,#3634,#3635));
#1138=EDGE_LOOP('',(#3636));
#1139=EDGE_LOOP('',(#3637));
#1140=EDGE_LOOP('',(#3638,#3639,#3640,#3641));
#1141=EDGE_LOOP('',(#3642));
#1142=EDGE_LOOP('',(#3643));
#1143=EDGE_LOOP('',(#3644,#3645,#3646,#3647));
#1144=EDGE_LOOP('',(#3648,#3649,#3650,#3651));
#1145=EDGE_LOOP('',(#3652,#3653,#3654,#3655));
#1146=EDGE_LOOP('',(#3656,#3657,#3658,#3659));
#1147=EDGE_LOOP('',(#3660,#3661,#3662,#3663));
#1148=EDGE_LOOP('',(#3664));
#1149=EDGE_LOOP('',(#3665));
#1150=EDGE_LOOP('',(#3666,#3667,#3668,#3669));
#1151=EDGE_LOOP('',(#3670,#3671,#3672,#3673));
#1152=EDGE_LOOP('',(#3674));
#1153=EDGE_LOOP('',(#3675));
#1154=EDGE_LOOP('',(#3676));
#1155=EDGE_LOOP('',(#3677));
#1156=EDGE_LOOP('',(#3678));
#1157=EDGE_LOOP('',(#3679));
#1158=EDGE_LOOP('',(#3680));
#1159=EDGE_LOOP('',(#3681));
#1160=EDGE_LOOP('',(#3682));
#1161=EDGE_LOOP('',(#3683));
#1162=EDGE_LOOP('',(#3684));
#1163=EDGE_LOOP('',(#3685));
#1164=EDGE_LOOP('',(#3686,#3687,#3688,#3689));
#1165=EDGE_LOOP('',(#3690,#3691,#3692,#3693));
#1166=EDGE_LOOP('',(#3694));
#1167=EDGE_LOOP('',(#3695));
#1168=EDGE_LOOP('',(#3696));
#1169=EDGE_LOOP('',(#3697));
#1170=EDGE_LOOP('',(#3698,#3699,#3700,#3701));
#1171=EDGE_LOOP('',(#3702));
#1172=EDGE_LOOP('',(#3703));
#1173=EDGE_LOOP('',(#3704,#3705,#3706,#3707));
#1174=EDGE_LOOP('',(#3708));
#1175=EDGE_LOOP('',(#3709,#3710,#3711,#3712,#3713,#3714));
#1176=EDGE_LOOP('',(#3715,#3716,#3717,#3718));
#1177=EDGE_LOOP('',(#3719,#3720,#3721,#3722));
#1178=EDGE_LOOP('',(#3723,#3724,#3725,#3726,#3727,#3728));
#1179=EDGE_LOOP('',(#3729,#3730,#3731,#3732,#3733,#3734));
#1180=EDGE_LOOP('',(#3735,#3736,#3737,#3738));
#1181=EDGE_LOOP('',(#3739,#3740,#3741,#3742));
#1182=EDGE_LOOP('',(#3743,#3744,#3745,#3746));
#1183=EDGE_LOOP('',(#3747,#3748,#3749,#3750));
#1184=EDGE_LOOP('',(#3751));
#1185=EDGE_LOOP('',(#3752,#3753,#3754,#3755));
#1186=EDGE_LOOP('',(#3756,#3757));
#1187=EDGE_LOOP('',(#3758,#3759,#3760,#3761,#3762,#3763,#3764));
#1188=EDGE_LOOP('',(#3765,#3766,#3767,#3768,#3769));
#1189=EDGE_LOOP('',(#3770,#3771,#3772,#3773));
#1190=EDGE_LOOP('',(#3774));
#1191=EDGE_LOOP('',(#3775));
#1192=EDGE_LOOP('',(#3776,#3777,#3778,#3779));
#1193=EDGE_LOOP('',(#3780,#3781));
#1194=EDGE_LOOP('',(#3782));
#1195=EDGE_LOOP('',(#3783,#3784,#3785,#3786,#3787,#3788,#3789));
#1196=EDGE_LOOP('',(#3790,#3791,#3792,#3793));
#1197=EDGE_LOOP('',(#3794));
#1198=EDGE_LOOP('',(#3795));
#1199=EDGE_LOOP('',(#3796,#3797,#3798,#3799,#3800,#3801));
#1200=EDGE_LOOP('',(#3802,#3803,#3804,#3805));
#1201=EDGE_LOOP('',(#3806,#3807,#3808,#3809));
#1202=EDGE_LOOP('',(#3810,#3811,#3812,#3813));
#1203=EDGE_LOOP('',(#3814,#3815,#3816,#3817));
#1204=EDGE_LOOP('',(#3818,#3819,#3820,#3821));
#1205=EDGE_LOOP('',(#3822));
#1206=EDGE_LOOP('',(#3823));
#1207=EDGE_LOOP('',(#3824));
#1208=EDGE_LOOP('',(#3825));
#1209=EDGE_LOOP('',(#3826));
#1210=EDGE_LOOP('',(#3827));
#1211=EDGE_LOOP('',(#3828));
#1212=EDGE_LOOP('',(#3829));
#1213=EDGE_LOOP('',(#3830));
#1214=EDGE_LOOP('',(#3831));
#1215=EDGE_LOOP('',(#3832,#3833,#3834,#3835));
#1216=EDGE_LOOP('',(#3836,#3837,#3838,#3839));
#1217=EDGE_LOOP('',(#3840));
#1218=EDGE_LOOP('',(#3841));
#1219=EDGE_LOOP('',(#3842));
#1220=EDGE_LOOP('',(#3843));
#1221=EDGE_LOOP('',(#3844,#3845));
#1222=EDGE_LOOP('',(#3846,#3847,#3848,#3849,#3850,#3851,#3852,#3853));
#1223=EDGE_LOOP('',(#3854,#3855,#3856,#3857,#3858));
#1224=EDGE_LOOP('',(#3859,#3860,#3861,#3862,#3863,#3864,#3865));
#1225=EDGE_LOOP('',(#3866,#3867,#3868,#3869));
#1226=EDGE_LOOP('',(#3870));
#1227=EDGE_LOOP('',(#3871));
#1228=EDGE_LOOP('',(#3872,#3873,#3874,#3875));
#1229=EDGE_LOOP('',(#3876));
#1230=EDGE_LOOP('',(#3877));
#1231=EDGE_LOOP('',(#3878,#3879,#3880,#3881));
#1232=EDGE_LOOP('',(#3882));
#1233=EDGE_LOOP('',(#3883));
#1234=EDGE_LOOP('',(#3884));
#1235=EDGE_LOOP('',(#3885));
#1236=EDGE_LOOP('',(#3886,#3887,#3888,#3889));
#1237=EDGE_LOOP('',(#3890,#3891,#3892,#3893));
#1238=EDGE_LOOP('',(#3894,#3895,#3896,#3897));
#1239=EDGE_LOOP('',(#3898));
#1240=EDGE_LOOP('',(#3899));
#1241=EDGE_LOOP('',(#3900,#3901,#3902,#3903));
#1242=EDGE_LOOP('',(#3904));
#1243=EDGE_LOOP('',(#3905));
#1244=EDGE_LOOP('',(#3906));
#1245=EDGE_LOOP('',(#3907,#3908,#3909,#3910));
#1246=EDGE_LOOP('',(#3911,#3912,#3913,#3914));
#1247=EDGE_LOOP('',(#3915,#3916,#3917,#3918));
#1248=EDGE_LOOP('',(#3919,#3920,#3921,#3922));
#1249=EDGE_LOOP('',(#3923,#3924,#3925,#3926));
#1250=EDGE_LOOP('',(#3927));
#1251=EDGE_LOOP('',(#3928));
#1252=EDGE_LOOP('',(#3929));
#1253=EDGE_LOOP('',(#3930));
#1254=EDGE_LOOP('',(#3931));
#1255=EDGE_LOOP('',(#3932));
#1256=EDGE_LOOP('',(#3933));
#1257=EDGE_LOOP('',(#3934));
#1258=EDGE_LOOP('',(#3935));
#1259=EDGE_LOOP('',(#3936));
#1260=EDGE_LOOP('',(#3937));
#1261=EDGE_LOOP('',(#3938));
#1262=EDGE_LOOP('',(#3939));
#1263=EDGE_LOOP('',(#3940,#3941,#3942,#3943));
#1264=EDGE_LOOP('',(#3944,#3945,#3946,#3947));
#1265=EDGE_LOOP('',(#3948));
#1266=EDGE_LOOP('',(#3949));
#1267=EDGE_LOOP('',(#3950));
#1268=EDGE_LOOP('',(#3951));
#1269=EDGE_LOOP('',(#3952,#3953,#3954,#3955));
#1270=EDGE_LOOP('',(#3956,#3957,#3958,#3959));
#1271=EDGE_LOOP('',(#3960));
#1272=EDGE_LOOP('',(#3961));
#1273=EDGE_LOOP('',(#3962));
#1274=EDGE_LOOP('',(#3963));
#1275=EDGE_LOOP('',(#3964,#3965,#3966,#3967));
#1276=EDGE_LOOP('',(#3968,#3969,#3970,#3971));
#1277=EDGE_LOOP('',(#3972));
#1278=EDGE_LOOP('',(#3973));
#1279=EDGE_LOOP('',(#3974));
#1280=EDGE_LOOP('',(#3975));
#1281=EDGE_LOOP('',(#3976,#3977,#3978,#3979));
#1282=EDGE_LOOP('',(#3980));
#1283=EDGE_LOOP('',(#3981));
#1284=EDGE_LOOP('',(#3982,#3983,#3984,#3985));
#1285=EDGE_LOOP('',(#3986));
#1286=EDGE_LOOP('',(#3987));
#1287=EDGE_LOOP('',(#3988,#3989,#3990,#3991));
#1288=EDGE_LOOP('',(#3992));
#1289=EDGE_LOOP('',(#3993));
#1290=EDGE_LOOP('',(#3994,#3995,#3996,#3997));
#1291=EDGE_LOOP('',(#3998));
#1292=EDGE_LOOP('',(#3999));
#1293=EDGE_LOOP('',(#4000,#4001,#4002,#4003));
#1294=EDGE_LOOP('',(#4004,#4005,#4006,#4007));
#1295=EDGE_LOOP('',(#4008,#4009,#4010,#4011));
#1296=EDGE_LOOP('',(#4012,#4013,#4014,#4015));
#1297=EDGE_LOOP('',(#4016,#4017,#4018,#4019));
#1298=EDGE_LOOP('',(#4020));
#1299=EDGE_LOOP('',(#4021));
#1300=EDGE_LOOP('',(#4022,#4023,#4024,#4025));
#1301=EDGE_LOOP('',(#4026));
#1302=EDGE_LOOP('',(#4027));
#1303=EDGE_LOOP('',(#4028,#4029,#4030,#4031));
#1304=EDGE_LOOP('',(#4032));
#1305=EDGE_LOOP('',(#4033));
#1306=EDGE_LOOP('',(#4034,#4035,#4036,#4037));
#1307=EDGE_LOOP('',(#4038));
#1308=EDGE_LOOP('',(#4039));
#1309=EDGE_LOOP('',(#4040,#4041,#4042,#4043));
#1310=EDGE_LOOP('',(#4044));
#1311=EDGE_LOOP('',(#4045));
#1312=EDGE_LOOP('',(#4046,#4047,#4048,#4049));
#1313=EDGE_LOOP('',(#4050));
#1314=EDGE_LOOP('',(#4051));
#1315=EDGE_LOOP('',(#4052,#4053,#4054,#4055));
#1316=EDGE_LOOP('',(#4056,#4057,#4058,#4059));
#1317=EDGE_LOOP('',(#4060,#4061,#4062,#4063));
#1318=EDGE_LOOP('',(#4064,#4065,#4066,#4067));
#1319=EDGE_LOOP('',(#4068,#4069,#4070,#4071));
#1320=EDGE_LOOP('',(#4072,#4073,#4074,#4075));
#1321=EDGE_LOOP('',(#4076));
#1322=EDGE_LOOP('',(#4077));
#1323=EDGE_LOOP('',(#4078,#4079,#4080,#4081));
#1324=EDGE_LOOP('',(#4082,#4083,#4084,#4085));
#1325=EDGE_LOOP('',(#4086));
#1326=EDGE_LOOP('',(#4087));
#1327=EDGE_LOOP('',(#4088,#4089,#4090,#4091));
#1328=EDGE_LOOP('',(#4092,#4093,#4094,#4095));
#1329=EDGE_LOOP('',(#4096));
#1330=EDGE_LOOP('',(#4097,#4098,#4099,#4100));
#1331=EDGE_LOOP('',(#4101,#4102,#4103,#4104));
#1332=EDGE_LOOP('',(#4105,#4106,#4107,#4108));
#1333=EDGE_LOOP('',(#4109));
#1334=EDGE_LOOP('',(#4110));
#1335=EDGE_LOOP('',(#4111,#4112,#4113,#4114));
#1336=EDGE_LOOP('',(#4115,#4116,#4117,#4118));
#1337=EDGE_LOOP('',(#4119,#4120,#4121,#4122));
#1338=EDGE_LOOP('',(#4123));
#1339=EDGE_LOOP('',(#4124,#4125,#4126,#4127));
#1340=EDGE_LOOP('',(#4128,#4129,#4130,#4131));
#1341=EDGE_LOOP('',(#4132,#4133,#4134,#4135));
#1342=EDGE_LOOP('',(#4136,#4137,#4138,#4139));
#1343=EDGE_LOOP('',(#4140,#4141,#4142,#4143));
#1344=EDGE_LOOP('',(#4144,#4145,#4146,#4147));
#1345=EDGE_LOOP('',(#4148,#4149,#4150,#4151,#4152,#4153));
#1346=EDGE_LOOP('',(#4154,#4155,#4156,#4157,#4158,#4159));
#1347=EDGE_LOOP('',(#4160,#4161,#4162,#4163));
#1348=EDGE_LOOP('',(#4164));
#1349=EDGE_LOOP('',(#4165));
#1350=EDGE_LOOP('',(#4166,#4167,#4168,#4169,#4170,#4171));
#1351=EDGE_LOOP('',(#4172));
#1352=EDGE_LOOP('',(#4173,#4174,#4175,#4176,#4177,#4178));
#1353=EDGE_LOOP('',(#4179));
#1354=EDGE_LOOP('',(#4180,#4181,#4182,#4183));
#1355=EDGE_LOOP('',(#4184,#4185,#4186,#4187));
#1356=EDGE_LOOP('',(#4188,#4189,#4190,#4191));
#1357=EDGE_LOOP('',(#4192,#4193,#4194,#4195));
#1358=EDGE_LOOP('',(#4196,#4197,#4198,#4199));
#1359=EDGE_LOOP('',(#4200,#4201,#4202,#4203));
#1360=EDGE_LOOP('',(#4204));
#1361=EDGE_LOOP('',(#4205));
#1362=EDGE_LOOP('',(#4206,#4207,#4208,#4209));
#1363=EDGE_LOOP('',(#4210));
#1364=EDGE_LOOP('',(#4211));
#1365=EDGE_LOOP('',(#4212,#4213,#4214,#4215));
#1366=EDGE_LOOP('',(#4216,#4217,#4218,#4219));
#1367=EDGE_LOOP('',(#4220));
#1368=EDGE_LOOP('',(#4221));
#1369=EDGE_LOOP('',(#4222,#4223,#4224,#4225));
#1370=EDGE_LOOP('',(#4226));
#1371=EDGE_LOOP('',(#4227));
#1372=EDGE_LOOP('',(#4228,#4229,#4230,#4231));
#1373=EDGE_LOOP('',(#4232));
#1374=EDGE_LOOP('',(#4233));
#1375=EDGE_LOOP('',(#4234,#4235,#4236,#4237));
#1376=EDGE_LOOP('',(#4238));
#1377=EDGE_LOOP('',(#4239));
#1378=EDGE_LOOP('',(#4240,#4241,#4242,#4243));
#1379=EDGE_LOOP('',(#4244,#4245,#4246,#4247));
#1380=EDGE_LOOP('',(#4248,#4249,#4250,#4251));
#1381=EDGE_LOOP('',(#4252));
#1382=EDGE_LOOP('',(#4253));
#1383=EDGE_LOOP('',(#4254,#4255,#4256,#4257));
#1384=EDGE_LOOP('',(#4258));
#1385=EDGE_LOOP('',(#4259));
#1386=EDGE_LOOP('',(#4260,#4261,#4262,#4263,#4264,#4265,#4266,#4267,#4268));
#1387=EDGE_LOOP('',(#4269,#4270,#4271,#4272,#4273,#4274,#4275,#4276,#4277));
#1388=EDGE_LOOP('',(#4278,#4279,#4280,#4281));
#1389=EDGE_LOOP('',(#4282,#4283,#4284,#4285));
#1390=EDGE_LOOP('',(#4286,#4287,#4288,#4289));
#1391=EDGE_LOOP('',(#4290,#4291,#4292,#4293));
#1392=EDGE_LOOP('',(#4294,#4295,#4296,#4297));
#1393=EDGE_LOOP('',(#4298,#4299,#4300,#4301));
#1394=EDGE_LOOP('',(#4302,#4303,#4304,#4305));
#1395=EDGE_LOOP('',(#4306));
#1396=EDGE_LOOP('',(#4307));
#1397=EDGE_LOOP('',(#4308));
#1398=EDGE_LOOP('',(#4309));
#1399=EDGE_LOOP('',(#4310,#4311,#4312,#4313));
#1400=EDGE_LOOP('',(#4314));
#1401=EDGE_LOOP('',(#4315));
#1402=EDGE_LOOP('',(#4316,#4317,#4318,#4319));
#1403=EDGE_LOOP('',(#4320,#4321,#4322,#4323));
#1404=EDGE_LOOP('',(#4324,#4325,#4326,#4327));
#1405=EDGE_LOOP('',(#4328,#4329,#4330,#4331));
#1406=EDGE_LOOP('',(#4332,#4333,#4334,#4335));
#1407=EDGE_LOOP('',(#4336,#4337,#4338,#4339,#4340,#4341));
#1408=EDGE_LOOP('',(#4342));
#1409=EDGE_LOOP('',(#4343,#4344,#4345,#4346,#4347,#4348));
#1410=EDGE_LOOP('',(#4349,#4350,#4351,#4352,#4353,#4354,#4355,#4356,#4357,
#4358,#4359,#4360));
#1411=EDGE_LOOP('',(#4361,#4362));
#1412=EDGE_LOOP('',(#4363,#4364,#4365,#4366,#4367,#4368,#4369,#4370,#4371));
#1413=EDGE_LOOP('',(#4372,#4373));
#1414=EDGE_LOOP('',(#4374,#4375,#4376,#4377,#4378));
#1415=EDGE_LOOP('',(#4379,#4380,#4381,#4382,#4383,#4384,#4385,#4386,#4387,
#4388,#4389,#4390));
#1416=EDGE_LOOP('',(#4391,#4392,#4393,#4394,#4395));
#1417=EDGE_LOOP('',(#4396,#4397,#4398,#4399,#4400,#4401,#4402,#4403,#4404,
#4405));
#1418=EDGE_LOOP('',(#4406,#4407,#4408,#4409));
#1419=EDGE_LOOP('',(#4410,#4411,#4412,#4413));
#1420=EDGE_LOOP('',(#4414,#4415,#4416,#4417,#4418,#4419,#4420,#4421));
#1421=EDGE_LOOP('',(#4422,#4423));
#1422=EDGE_LOOP('',(#4424));
#1423=EDGE_LOOP('',(#4425));
#1424=EDGE_LOOP('',(#4426,#4427,#4428,#4429,#4430));
#1425=EDGE_LOOP('',(#4431,#4432,#4433,#4434,#4435,#4436,#4437,#4438));
#1426=EDGE_LOOP('',(#4439));
#1427=EDGE_LOOP('',(#4440,#4441,#4442,#4443));
#1428=EDGE_LOOP('',(#4444,#4445,#4446,#4447));
#1429=EDGE_LOOP('',(#4448,#4449,#4450,#4451));
#1430=EDGE_LOOP('',(#4452));
#1431=EDGE_LOOP('',(#4453,#4454,#4455,#4456));
#1432=EDGE_LOOP('',(#4457));
#1433=EDGE_LOOP('',(#4458,#4459,#4460,#4461));
#1434=EDGE_LOOP('',(#4462));
#1435=EDGE_LOOP('',(#4463));
#1436=EDGE_LOOP('',(#4464));
#1437=EDGE_LOOP('',(#4465));
#1438=EDGE_LOOP('',(#4466,#4467,#4468,#4469));
#1439=EDGE_LOOP('',(#4470));
#1440=EDGE_LOOP('',(#4471));
#1441=EDGE_LOOP('',(#4472));
#1442=EDGE_LOOP('',(#4473));
#1443=EDGE_LOOP('',(#4474,#4475,#4476,#4477));
#1444=EDGE_LOOP('',(#4478,#4479,#4480,#4481));
#1445=EDGE_LOOP('',(#4482,#4483,#4484,#4485));
#1446=EDGE_LOOP('',(#4486));
#1447=EDGE_LOOP('',(#4487));
#1448=EDGE_LOOP('',(#4488));
#1449=EDGE_LOOP('',(#4489));
#1450=EDGE_LOOP('',(#4490,#4491,#4492,#4493));
#1451=EDGE_LOOP('',(#4494,#4495,#4496,#4497));
#1452=EDGE_LOOP('',(#4498));
#1453=EDGE_LOOP('',(#4499));
#1454=EDGE_LOOP('',(#4500));
#1455=EDGE_LOOP('',(#4501));
#1456=EDGE_LOOP('',(#4502));
#1457=EDGE_LOOP('',(#4503,#4504,#4505,#4506));
#1458=EDGE_LOOP('',(#4507,#4508,#4509,#4510));
#1459=EDGE_LOOP('',(#4511));
#1460=EDGE_LOOP('',(#4512));
#1461=EDGE_LOOP('',(#4513,#4514,#4515,#4516));
#1462=EDGE_LOOP('',(#4517,#4518,#4519,#4520));
#1463=EDGE_LOOP('',(#4521,#4522,#4523,#4524));
#1464=EDGE_LOOP('',(#4525,#4526,#4527,#4528));
#1465=EDGE_LOOP('',(#4529,#4530,#4531,#4532));
#1466=EDGE_LOOP('',(#4533,#4534,#4535,#4536));
#1467=EDGE_LOOP('',(#4537,#4538,#4539,#4540,#4541,#4542));
#1468=EDGE_LOOP('',(#4543));
#1469=EDGE_LOOP('',(#4544,#4545,#4546,#4547,#4548,#4549));
#1470=EDGE_LOOP('',(#4550,#4551,#4552,#4553));
#1471=EDGE_LOOP('',(#4554,#4555,#4556,#4557));
#1472=EDGE_LOOP('',(#4558));
#1473=EDGE_LOOP('',(#4559,#4560,#4561,#4562));
#1474=EDGE_LOOP('',(#4563,#4564,#4565,#4566));
#1475=EDGE_LOOP('',(#4567,#4568,#4569,#4570));
#1476=EDGE_LOOP('',(#4571));
#1477=EDGE_LOOP('',(#4572));
#1478=EDGE_LOOP('',(#4573,#4574,#4575,#4576));
#1479=EDGE_LOOP('',(#4577,#4578,#4579,#4580));
#1480=EDGE_LOOP('',(#4581,#4582,#4583,#4584));
#1481=EDGE_LOOP('',(#4585));
#1482=EDGE_LOOP('',(#4586,#4587,#4588,#4589));
#1483=EDGE_LOOP('',(#4590,#4591,#4592,#4593));
#1484=EDGE_LOOP('',(#4594,#4595,#4596,#4597));
#1485=EDGE_LOOP('',(#4598,#4599,#4600,#4601));
#1486=EDGE_LOOP('',(#4602,#4603,#4604,#4605));
#1487=EDGE_LOOP('',(#4606,#4607,#4608,#4609));
#1488=EDGE_LOOP('',(#4610,#4611,#4612,#4613,#4614,#4615));
#1489=EDGE_LOOP('',(#4616,#4617,#4618,#4619,#4620,#4621));
#1490=LINE('',#7745,#1825);
#1491=LINE('',#7751,#1826);
#1492=LINE('',#7757,#1827);
#1493=LINE('',#7763,#1828);
#1494=LINE('',#7769,#1829);
#1495=LINE('',#7775,#1830);
#1496=LINE('',#7781,#1831);
#1497=LINE('',#7787,#1832);
#1498=LINE('',#7793,#1833);
#1499=LINE('',#7798,#1834);
#1500=LINE('',#7800,#1835);
#1501=LINE('',#7802,#1836);
#1502=LINE('',#7803,#1837);
#1503=LINE('',#7806,#1838);
#1504=LINE('',#7808,#1839);
#1505=LINE('',#7809,#1840);
#1506=LINE('',#7812,#1841);
#1507=LINE('',#7814,#1842);
#1508=LINE('',#7815,#1843);
#1509=LINE('',#7817,#1844);
#1510=LINE('',#7818,#1845);
#1511=LINE('',#7825,#1846);
#1512=LINE('',#7827,#1847);
#1513=LINE('',#7829,#1848);
#1514=LINE('',#7830,#1849);
#1515=LINE('',#7833,#1850);
#1516=LINE('',#7835,#1851);
#1517=LINE('',#7836,#1852);
#1518=LINE('',#7839,#1853);
#1519=LINE('',#7841,#1854);
#1520=LINE('',#7842,#1855);
#1521=LINE('',#7844,#1856);
#1522=LINE('',#7845,#1857);
#1523=LINE('',#7852,#1858);
#1524=LINE('',#7854,#1859);
#1525=LINE('',#7856,#1860);
#1526=LINE('',#7857,#1861);
#1527=LINE('',#7860,#1862);
#1528=LINE('',#7862,#1863);
#1529=LINE('',#7863,#1864);
#1530=LINE('',#7866,#1865);
#1531=LINE('',#7868,#1866);
#1532=LINE('',#7869,#1867);
#1533=LINE('',#7871,#1868);
#1534=LINE('',#7872,#1869);
#1535=LINE('',#7880,#1870);
#1536=LINE('',#7887,#1871);
#1537=LINE('',#7894,#1872);
#1538=LINE('',#7901,#1873);
#1539=LINE('',#7908,#1874);
#1540=LINE('',#7915,#1875);
#1541=LINE('',#7922,#1876);
#1542=LINE('',#7929,#1877);
#1543=LINE('',#7936,#1878);
#1544=LINE('',#7944,#1879);
#1545=LINE('',#7948,#1880);
#1546=LINE('',#7950,#1881);
#1547=LINE('',#7952,#1882);
#1548=LINE('',#7953,#1883);
#1549=LINE('',#7956,#1884);
#1550=LINE('',#7958,#1885);
#1551=LINE('',#7959,#1886);
#1552=LINE('',#7962,#1887);
#1553=LINE('',#7964,#1888);
#1554=LINE('',#7965,#1889);
#1555=LINE('',#7967,#1890);
#1556=LINE('',#7968,#1891);
#1557=LINE('',#7976,#1892);
#1558=LINE('',#7985,#1893);
#1559=LINE('',#7994,#1894);
#1560=LINE('',#8003,#1895);
#1561=LINE('',#8011,#1896);
#1562=LINE('',#8015,#1897);
#1563=LINE('',#8019,#1898);
#1564=LINE('',#8023,#1899);
#1565=LINE('',#8028,#1900);
#1566=LINE('',#8036,#1901);
#1567=LINE('',#8041,#1902);
#1568=LINE('',#8050,#1903);
#1569=LINE('',#8056,#1904);
#1570=LINE('',#8908,#1905);
#1571=LINE('',#8914,#1906);
#1572=LINE('',#8916,#1907);
#1573=LINE('',#8918,#1908);
#1574=LINE('',#8920,#1909);
#1575=LINE('',#8922,#1910);
#1576=LINE('',#8923,#1911);
#1577=LINE('',#8926,#1912);
#1578=LINE('',#8928,#1913);
#1579=LINE('',#8929,#1914);
#1580=LINE('',#8932,#1915);
#1581=LINE('',#8933,#1916);
#1582=LINE('',#8937,#1917);
#1583=LINE('',#8939,#1918);
#1584=LINE('',#8940,#1919);
#1585=LINE('',#8941,#1920);
#1586=LINE('',#8944,#1921);
#1587=LINE('',#8945,#1922);
#1588=LINE('',#8946,#1923);
#1589=LINE('',#8949,#1924);
#1590=LINE('',#8950,#1925);
#1591=LINE('',#8952,#1926);
#1592=LINE('',#8959,#1927);
#1593=LINE('',#8963,#1928);
#1594=LINE('',#8993,#1929);
#1595=LINE('',#8997,#1930);
#1596=LINE('',#9018,#1931);
#1597=LINE('',#9020,#1932);
#1598=LINE('',#9029,#1933);
#1599=LINE('',#9043,#1934);
#1600=LINE('',#9051,#1935);
#1601=LINE('',#9057,#1936);
#1602=LINE('',#9063,#1937);
#1603=LINE('',#9068,#1938);
#1604=LINE('',#9074,#1939);
#1605=LINE('',#9080,#1940);
#1606=LINE('',#9086,#1941);
#1607=LINE('',#9095,#1942);
#1608=LINE('',#9101,#1943);
#1609=LINE('',#9109,#1944);
#1610=LINE('',#9115,#1945);
#1611=LINE('',#9125,#1946);
#1612=LINE('',#9127,#1947);
#1613=LINE('',#9163,#1948);
#1614=LINE('',#9169,#1949);
#1615=LINE('',#9176,#1950);
#1616=LINE('',#9216,#1951);
#1617=LINE('',#9227,#1952);
#1618=LINE('',#9230,#1953);
#1619=LINE('',#9236,#1954);
#1620=LINE('',#9243,#1955);
#1621=LINE('',#9250,#1956);
#1622=LINE('',#9256,#1957);
#1623=LINE('',#9262,#1958);
#1624=LINE('',#9268,#1959);
#1625=LINE('',#9274,#1960);
#1626=LINE('',#9283,#1961);
#1627=LINE('',#9289,#1962);
#1628=LINE('',#9298,#1963);
#1629=LINE('',#9304,#1964);
#1630=LINE('',#9313,#1965);
#1631=LINE('',#9319,#1966);
#1632=LINE('',#9328,#1967);
#1633=LINE('',#9337,#1968);
#1634=LINE('',#9346,#1969);
#1635=LINE('',#9355,#1970);
#1636=LINE('',#9366,#1971);
#1637=LINE('',#9368,#1972);
#1638=LINE('',#9369,#1973);
#1639=LINE('',#9372,#1974);
#1640=LINE('',#9374,#1975);
#1641=LINE('',#9375,#1976);
#1642=LINE('',#9380,#1977);
#1643=LINE('',#9381,#1978);
#1644=LINE('',#9383,#1979);
#1645=LINE('',#9384,#1980);
#1646=LINE('',#9394,#1981);
#1647=LINE('',#9401,#1982);
#1648=LINE('',#9408,#1983);
#1649=LINE('',#9415,#1984);
#1650=LINE('',#9422,#1985);
#1651=LINE('',#9427,#1986);
#1652=LINE('',#9434,#1987);
#1653=LINE('',#9437,#1988);
#1654=LINE('',#9440,#1989);
#1655=LINE('',#9442,#1990);
#1656=LINE('',#9443,#1991);
#1657=LINE('',#9449,#1992);
#1658=LINE('',#9451,#1993);
#1659=LINE('',#9452,#1994);
#1660=LINE('',#9461,#1995);
#1661=LINE('',#9466,#1996);
#1662=LINE('',#9476,#1997);
#1663=LINE('',#9480,#1998);
#1664=LINE('',#9484,#1999);
#1665=LINE('',#9491,#2000);
#1666=LINE('',#9495,#2001);
#1667=LINE('',#9499,#2002);
#1668=LINE('',#9504,#2003);
#1669=LINE('',#9506,#2004);
#1670=LINE('',#9508,#2005);
#1671=LINE('',#9509,#2006);
#1672=LINE('',#9512,#2007);
#1673=LINE('',#9514,#2008);
#1674=LINE('',#9515,#2009);
#1675=LINE('',#9518,#2010);
#1676=LINE('',#9520,#2011);
#1677=LINE('',#9521,#2012);
#1678=LINE('',#9524,#2013);
#1679=LINE('',#9526,#2014);
#1680=LINE('',#9527,#2015);
#1681=LINE('',#9530,#2016);
#1682=LINE('',#9532,#2017);
#1683=LINE('',#9533,#2018);
#1684=LINE('',#9535,#2019);
#1685=LINE('',#9536,#2020);
#1686=LINE('',#9545,#2021);
#1687=LINE('',#9553,#2022);
#1688=LINE('',#9555,#2023);
#1689=LINE('',#9557,#2024);
#1690=LINE('',#9559,#2025);
#1691=LINE('',#9561,#2026);
#1692=LINE('',#9562,#2027);
#1693=LINE('',#9568,#2028);
#1694=LINE('',#9570,#2029);
#1695=LINE('',#9572,#2030);
#1696=LINE('',#9574,#2031);
#1697=LINE('',#9576,#2032);
#1698=LINE('',#9577,#2033);
#1699=LINE('',#9581,#2034);
#1700=LINE('',#9582,#2035);
#1701=LINE('',#9584,#2036);
#1702=LINE('',#9586,#2037);
#1703=LINE('',#9588,#2038);
#1704=LINE('',#9590,#2039);
#1705=LINE('',#9597,#2040);
#1706=LINE('',#9603,#2041);
#1707=LINE('',#9607,#2042);
#1708=LINE('',#9612,#2043);
#1709=LINE('',#9622,#2044);
#1710=LINE('',#9629,#2045);
#1711=LINE('',#9634,#2046);
#1712=LINE('',#9642,#2047);
#1713=LINE('',#9646,#2048);
#1714=LINE('',#9653,#2049);
#1715=LINE('',#9668,#2050);
#1716=LINE('',#9689,#2051);
#1717=LINE('',#9714,#2052);
#1718=LINE('',#9715,#2053);
#1719=LINE('',#9717,#2054);
#1720=LINE('',#9719,#2055);
#1721=LINE('',#9724,#2056);
#1722=LINE('',#9727,#2057);
#1723=LINE('',#9729,#2058);
#1724=LINE('',#9739,#2059);
#1725=LINE('',#9747,#2060);
#1726=LINE('',#9751,#2061);
#1727=LINE('',#9753,#2062);
#1728=LINE('',#9755,#2063);
#1729=LINE('',#9756,#2064);
#1730=LINE('',#9759,#2065);
#1731=LINE('',#9761,#2066);
#1732=LINE('',#9762,#2067);
#1733=LINE('',#9765,#2068);
#1734=LINE('',#9767,#2069);
#1735=LINE('',#9768,#2070);
#1736=LINE('',#9772,#2071);
#1737=LINE('',#9773,#2072);
#1738=LINE('',#9774,#2073);
#1739=LINE('',#9777,#2074);
#1740=LINE('',#9778,#2075);
#1741=LINE('',#9781,#2076);
#1742=LINE('',#9783,#2077);
#1743=LINE('',#9785,#2078);
#1744=LINE('',#9786,#2079);
#1745=LINE('',#9789,#2080);
#1746=LINE('',#9791,#2081);
#1747=LINE('',#9793,#2082);
#1748=LINE('',#9795,#2083);
#1749=LINE('',#9797,#2084);
#1750=LINE('',#9799,#2085);
#1751=LINE('',#9801,#2086);
#1752=LINE('',#9803,#2087);
#1753=LINE('',#9804,#2088);
#1754=LINE('',#9808,#2089);
#1755=LINE('',#9838,#2090);
#1756=LINE('',#9885,#2091);
#1757=LINE('',#9890,#2092);
#1758=LINE('',#9897,#2093);
#1759=LINE('',#9899,#2094);
#1760=LINE('',#9902,#2095);
#1761=LINE('',#9906,#2096);
#1762=LINE('',#9907,#2097);
#1763=LINE('',#9909,#2098);
#1764=LINE('',#9911,#2099);
#1765=LINE('',#9913,#2100);
#1766=LINE('',#9914,#2101);
#1767=LINE('',#9925,#2102);
#1768=LINE('',#9929,#2103);
#1769=LINE('',#9932,#2104);
#1770=LINE('',#9939,#2105);
#1771=LINE('',#9946,#2106);
#1772=LINE('',#9953,#2107);
#1773=LINE('',#9962,#2108);
#1774=LINE('',#9972,#2109);
#1775=LINE('',#9978,#2110);
#1776=LINE('',#9983,#2111);
#1777=LINE('',#9991,#2112);
#1778=LINE('',#9997,#2113);
#1779=LINE('',#10009,#2114);
#1780=LINE('',#10012,#2115);
#1781=LINE('',#10021,#2116);
#1782=LINE('',#10023,#2117);
#1783=LINE('',#10025,#2118);
#1784=LINE('',#10026,#2119);
#1785=LINE('',#10029,#2120);
#1786=LINE('',#10031,#2121);
#1787=LINE('',#10032,#2122);
#1788=LINE('',#10035,#2123);
#1789=LINE('',#10037,#2124);
#1790=LINE('',#10038,#2125);
#1791=LINE('',#10041,#2126);
#1792=LINE('',#10043,#2127);
#1793=LINE('',#10044,#2128);
#1794=LINE('',#10047,#2129);
#1795=LINE('',#10049,#2130);
#1796=LINE('',#10050,#2131);
#1797=LINE('',#10052,#2132);
#1798=LINE('',#10053,#2133);
#1799=LINE('',#10061,#2134);
#1800=LINE('',#10063,#2135);
#1801=LINE('',#10071,#2136);
#1802=LINE('',#10075,#2137);
#1803=LINE('',#10079,#2138);
#1804=LINE('',#10086,#2139);
#1805=LINE('',#10090,#2140);
#1806=LINE('',#10094,#2141);
#1807=LINE('',#10099,#2142);
#1808=LINE('',#10101,#2143);
#1809=LINE('',#10103,#2144);
#1810=LINE('',#10104,#2145);
#1811=LINE('',#10107,#2146);
#1812=LINE('',#10109,#2147);
#1813=LINE('',#10110,#2148);
#1814=LINE('',#10113,#2149);
#1815=LINE('',#10115,#2150);
#1816=LINE('',#10116,#2151);
#1817=LINE('',#10119,#2152);
#1818=LINE('',#10121,#2153);
#1819=LINE('',#10122,#2154);
#1820=LINE('',#10125,#2155);
#1821=LINE('',#10127,#2156);
#1822=LINE('',#10128,#2157);
#1823=LINE('',#10130,#2158);
#1824=LINE('',#10131,#2159);
#1825=VECTOR('',#6099,0.275);
#1826=VECTOR('',#6106,0.275);
#1827=VECTOR('',#6113,0.275);
#1828=VECTOR('',#6120,0.275);
#1829=VECTOR('',#6127,0.275);
#1830=VECTOR('',#6134,0.275);
#1831=VECTOR('',#6141,0.275);
#1832=VECTOR('',#6148,0.275);
#1833=VECTOR('',#6155,0.275);
#1834=VECTOR('',#6160,1.);
#1835=VECTOR('',#6161,1.);
#1836=VECTOR('',#6162,1.);
#1837=VECTOR('',#6163,1.);
#1838=VECTOR('',#6166,1.);
#1839=VECTOR('',#6167,1.);
#1840=VECTOR('',#6168,1.);
#1841=VECTOR('',#6171,1.);
#1842=VECTOR('',#6172,1.);
#1843=VECTOR('',#6173,1.);
#1844=VECTOR('',#6176,1.);
#1845=VECTOR('',#6177,1.);
#1846=VECTOR('',#6186,1.);
#1847=VECTOR('',#6187,1.);
#1848=VECTOR('',#6188,1.);
#1849=VECTOR('',#6189,1.);
#1850=VECTOR('',#6192,1.);
#1851=VECTOR('',#6193,1.);
#1852=VECTOR('',#6194,1.);
#1853=VECTOR('',#6197,1.);
#1854=VECTOR('',#6198,1.);
#1855=VECTOR('',#6199,1.);
#1856=VECTOR('',#6202,1.);
#1857=VECTOR('',#6203,1.);
#1858=VECTOR('',#6212,1.);
#1859=VECTOR('',#6213,1.);
#1860=VECTOR('',#6214,1.);
#1861=VECTOR('',#6215,1.);
#1862=VECTOR('',#6218,1.);
#1863=VECTOR('',#6219,1.);
#1864=VECTOR('',#6220,1.);
#1865=VECTOR('',#6223,1.);
#1866=VECTOR('',#6224,1.);
#1867=VECTOR('',#6225,1.);
#1868=VECTOR('',#6228,1.);
#1869=VECTOR('',#6229,1.);
#1870=VECTOR('',#6240,0.165);
#1871=VECTOR('',#6249,0.165);
#1872=VECTOR('',#6258,0.165);
#1873=VECTOR('',#6267,0.165);
#1874=VECTOR('',#6276,0.21);
#1875=VECTOR('',#6285,0.21);
#1876=VECTOR('',#6294,0.21);
#1877=VECTOR('',#6303,0.21);
#1878=VECTOR('',#6312,1.05);
#1879=VECTOR('',#6323,0.625);
#1880=VECTOR('',#6326,1.);
#1881=VECTOR('',#6327,1.);
#1882=VECTOR('',#6328,1.);
#1883=VECTOR('',#6329,1.);
#1884=VECTOR('',#6332,1.);
#1885=VECTOR('',#6333,1.);
#1886=VECTOR('',#6334,1.);
#1887=VECTOR('',#6337,1.);
#1888=VECTOR('',#6338,1.);
#1889=VECTOR('',#6339,1.);
#1890=VECTOR('',#6342,1.);
#1891=VECTOR('',#6343,1.);
#1892=VECTOR('',#6354,0.375);
#1893=VECTOR('',#6365,0.375);
#1894=VECTOR('',#6376,0.375);
#1895=VECTOR('',#6387,0.375);
#1896=VECTOR('',#6398,0.225);
#1897=VECTOR('',#6403,0.225);
#1898=VECTOR('',#6408,0.225);
#1899=VECTOR('',#6413,0.225);
#1900=VECTOR('',#6418,1.04);
#1901=VECTOR('',#6429,0.625);
#1902=VECTOR('',#6434,2.);
#1903=VECTOR('',#6447,0.625);
#1904=VECTOR('',#6454,0.8);
#1905=VECTOR('',#6477,0.21);
#1906=VECTOR('',#6484,1.);
#1907=VECTOR('',#6485,1.);
#1908=VECTOR('',#6486,1.);
#1909=VECTOR('',#6487,1.);
#1910=VECTOR('',#6488,1.);
#1911=VECTOR('',#6489,1.);
#1912=VECTOR('',#6492,1.);
#1913=VECTOR('',#6493,1.);
#1914=VECTOR('',#6494,1.);
#1915=VECTOR('',#6497,1.);
#1916=VECTOR('',#6498,1.);
#1917=VECTOR('',#6501,1.);
#1918=VECTOR('',#6502,1.);
#1919=VECTOR('',#6503,1.);
#1920=VECTOR('',#6504,1.);
#1921=VECTOR('',#6507,1.);
#1922=VECTOR('',#6508,1.);
#1923=VECTOR('',#6509,1.);
#1924=VECTOR('',#6512,1.);
#1925=VECTOR('',#6513,1.);
#1926=VECTOR('',#6516,1.);
#1927=VECTOR('',#6525,0.8);
#1928=VECTOR('',#6528,1.);
#1929=VECTOR('',#6531,1.);
#1930=VECTOR('',#6536,1.);
#1931=VECTOR('',#6537,0.2);
#1932=VECTOR('',#6540,1.);
#1933=VECTOR('',#6551,0.515);
#1934=VECTOR('',#6558,1.);
#1935=VECTOR('',#6569,2.4);
#1936=VECTOR('',#6576,1.25);
#1937=VECTOR('',#6585,1.);
#1938=VECTOR('',#6590,0.275);
#1939=VECTOR('',#6597,0.275);
#1940=VECTOR('',#6604,0.275);
#1941=VECTOR('',#6611,0.275);
#1942=VECTOR('',#6624,1.);
#1943=VECTOR('',#6631,1.25);
#1944=VECTOR('',#6642,1.);
#1945=VECTOR('',#6649,0.15);
#1946=VECTOR('',#6650,1.);
#1947=VECTOR('',#6651,1.);
#1948=VECTOR('',#6660,0.2);
#1949=VECTOR('',#6667,0.515);
#1950=VECTOR('',#6676,0.8);
#1951=VECTOR('',#6683,0.5);
#1952=VECTOR('',#6698,0.41);
#1953=VECTOR('',#6701,0.41);
#1954=VECTOR('',#6708,1.25);
#1955=VECTOR('',#6717,1.);
#1956=VECTOR('',#6726,0.275);
#1957=VECTOR('',#6733,0.275);
#1958=VECTOR('',#6740,0.275);
#1959=VECTOR('',#6747,0.275);
#1960=VECTOR('',#6754,2.4);
#1961=VECTOR('',#6767,1.);
#1962=VECTOR('',#6774,1.25);
#1963=VECTOR('',#6787,1.);
#1964=VECTOR('',#6794,1.25);
#1965=VECTOR('',#6807,0.4);
#1966=VECTOR('',#6814,0.5);
#1967=VECTOR('',#6827,0.25);
#1968=VECTOR('',#6840,0.25);
#1969=VECTOR('',#6853,0.25);
#1970=VECTOR('',#6866,0.25);
#1971=VECTOR('',#6881,1.);
#1972=VECTOR('',#6882,1.);
#1973=VECTOR('',#6883,1.);
#1974=VECTOR('',#6886,1.);
#1975=VECTOR('',#6887,1.);
#1976=VECTOR('',#6888,1.);
#1977=VECTOR('',#6893,1.);
#1978=VECTOR('',#6894,1.);
#1979=VECTOR('',#6897,1.);
#1980=VECTOR('',#6898,1.);
#1981=VECTOR('',#6911,1.05);
#1982=VECTOR('',#6920,1.);
#1983=VECTOR('',#6929,1.05);
#1984=VECTOR('',#6938,1.);
#1985=VECTOR('',#6947,1.05);
#1986=VECTOR('',#6954,0.9);
#1987=VECTOR('',#6961,1.);
#1988=VECTOR('',#6964,1.);
#1989=VECTOR('',#6967,1.);
#1990=VECTOR('',#6968,1.);
#1991=VECTOR('',#6969,1.);
#1992=VECTOR('',#6976,1.);
#1993=VECTOR('',#6979,1.);
#1994=VECTOR('',#6980,1.);
#1995=VECTOR('',#6991,0.895);
#1996=VECTOR('',#6998,0.605);
#1997=VECTOR('',#7013,0.4);
#1998=VECTOR('',#7018,0.425);
#1999=VECTOR('',#7023,0.41);
#2000=VECTOR('',#7032,0.26);
#2001=VECTOR('',#7037,0.25);
#2002=VECTOR('',#7042,0.225);
#2003=VECTOR('',#7047,1.);
#2004=VECTOR('',#7048,1.);
#2005=VECTOR('',#7049,1.);
#2006=VECTOR('',#7050,1.);
#2007=VECTOR('',#7053,1.);
#2008=VECTOR('',#7054,1.);
#2009=VECTOR('',#7055,1.);
#2010=VECTOR('',#7058,1.);
#2011=VECTOR('',#7059,1.);
#2012=VECTOR('',#7060,1.);
#2013=VECTOR('',#7063,1.);
#2014=VECTOR('',#7064,1.);
#2015=VECTOR('',#7065,1.);
#2016=VECTOR('',#7068,1.);
#2017=VECTOR('',#7069,1.);
#2018=VECTOR('',#7070,1.);
#2019=VECTOR('',#7073,1.);
#2020=VECTOR('',#7074,1.);
#2021=VECTOR('',#7087,0.43);
#2022=VECTOR('',#7096,1.);
#2023=VECTOR('',#7097,1.);
#2024=VECTOR('',#7098,1.);
#2025=VECTOR('',#7099,1.);
#2026=VECTOR('',#7100,1.);
#2027=VECTOR('',#7101,1.);
#2028=VECTOR('',#7106,1.);
#2029=VECTOR('',#7107,1.);
#2030=VECTOR('',#7108,1.);
#2031=VECTOR('',#7109,1.);
#2032=VECTOR('',#7110,1.);
#2033=VECTOR('',#7111,1.);
#2034=VECTOR('',#7116,1.);
#2035=VECTOR('',#7117,1.);
#2036=VECTOR('',#7120,1.);
#2037=VECTOR('',#7123,1.);
#2038=VECTOR('',#7126,1.);
#2039=VECTOR('',#7129,1.);
#2040=VECTOR('',#7138,0.46);
#2041=VECTOR('',#7147,0.525);
#2042=VECTOR('',#7152,0.515);
#2043=VECTOR('',#7159,0.2);
#2044=VECTOR('',#7172,0.475);
#2045=VECTOR('',#7181,0.355);
#2046=VECTOR('',#7188,0.31);
#2047=VECTOR('',#7199,0.275);
#2048=VECTOR('',#7204,0.265);
#2049=VECTOR('',#7213,0.5);
#2050=VECTOR('',#7222,0.47094010767585);
#2051=VECTOR('',#7229,0.47094010767585);
#2052=VECTOR('',#7232,1.);
#2053=VECTOR('',#7233,1.);
#2054=VECTOR('',#7236,1.);
#2055=VECTOR('',#7239,1.);
#2056=VECTOR('',#7244,0.25);
#2057=VECTOR('',#7249,1.);
#2058=VECTOR('',#7252,1.);
#2059=VECTOR('',#7267,0.4);
#2060=VECTOR('',#7278,0.225);
#2061=VECTOR('',#7281,1.);
#2062=VECTOR('',#7282,1.);
#2063=VECTOR('',#7283,1.);
#2064=VECTOR('',#7284,1.);
#2065=VECTOR('',#7287,1.);
#2066=VECTOR('',#7288,1.);
#2067=VECTOR('',#7289,1.);
#2068=VECTOR('',#7292,1.);
#2069=VECTOR('',#7293,1.);
#2070=VECTOR('',#7294,1.);
#2071=VECTOR('',#7297,1.);
#2072=VECTOR('',#7298,1.);
#2073=VECTOR('',#7299,1.);
#2074=VECTOR('',#7302,1.);
#2075=VECTOR('',#7303,1.);
#2076=VECTOR('',#7306,1.);
#2077=VECTOR('',#7307,1.);
#2078=VECTOR('',#7308,1.);
#2079=VECTOR('',#7309,1.);
#2080=VECTOR('',#7312,1.);
#2081=VECTOR('',#7313,1.);
#2082=VECTOR('',#7314,1.);
#2083=VECTOR('',#7315,1.);
#2084=VECTOR('',#7316,1.);
#2085=VECTOR('',#7317,1.);
#2086=VECTOR('',#7318,1.);
#2087=VECTOR('',#7319,1.);
#2088=VECTOR('',#7320,1.);
#2089=VECTOR('',#7323,1.);
#2090=VECTOR('',#7330,0.164999999999999);
#2091=VECTOR('',#7333,1.);
#2092=VECTOR('',#7338,1.);
#2093=VECTOR('',#7347,0.605);
#2094=VECTOR('',#7348,1.);
#2095=VECTOR('',#7351,1.);
#2096=VECTOR('',#7356,1.);
#2097=VECTOR('',#7357,1.);
#2098=VECTOR('',#7358,1.);
#2099=VECTOR('',#7359,1.);
#2100=VECTOR('',#7360,1.);
#2101=VECTOR('',#7361,1.);
#2102=VECTOR('',#7378,1.);
#2103=VECTOR('',#7385,1.);
#2104=VECTOR('',#7390,1.);
#2105=VECTOR('',#7399,0.165);
#2106=VECTOR('',#7408,0.165);
#2107=VECTOR('',#7417,0.4);
#2108=VECTOR('',#7430,0.94);
#2109=VECTOR('',#7443,0.99);
#2110=VECTOR('',#7450,0.225);
#2111=VECTOR('',#7457,0.99);
#2112=VECTOR('',#7468,0.94);
#2113=VECTOR('',#7475,1.);
#2114=VECTOR('',#7492,0.55);
#2115=VECTOR('',#7497,0.6);
#2116=VECTOR('',#7508,1.);
#2117=VECTOR('',#7509,1.);
#2118=VECTOR('',#7510,1.);
#2119=VECTOR('',#7511,1.);
#2120=VECTOR('',#7514,1.);
#2121=VECTOR('',#7515,1.);
#2122=VECTOR('',#7516,1.);
#2123=VECTOR('',#7519,1.);
#2124=VECTOR('',#7520,1.);
#2125=VECTOR('',#7521,1.);
#2126=VECTOR('',#7524,1.);
#2127=VECTOR('',#7525,1.);
#2128=VECTOR('',#7526,1.);
#2129=VECTOR('',#7529,1.);
#2130=VECTOR('',#7530,1.);
#2131=VECTOR('',#7531,1.);
#2132=VECTOR('',#7534,1.);
#2133=VECTOR('',#7535,1.);
#2134=VECTOR('',#7546,0.185);
#2135=VECTOR('',#7549,0.2);
#2136=VECTOR('',#7560,0.325);
#2137=VECTOR('',#7565,0.35);
#2138=VECTOR('',#7570,0.335);
#2139=VECTOR('',#7579,0.21);
#2140=VECTOR('',#7584,0.2);
#2141=VECTOR('',#7589,0.18);
#2142=VECTOR('',#7594,1.);
#2143=VECTOR('',#7595,1.);
#2144=VECTOR('',#7596,1.);
#2145=VECTOR('',#7597,1.);
#2146=VECTOR('',#7600,1.);
#2147=VECTOR('',#7601,1.);
#2148=VECTOR('',#7602,1.);
#2149=VECTOR('',#7605,1.);
#2150=VECTOR('',#7606,1.);
#2151=VECTOR('',#7607,1.);
#2152=VECTOR('',#7610,1.);
#2153=VECTOR('',#7611,1.);
#2154=VECTOR('',#7612,1.);
#2155=VECTOR('',#7615,1.);
#2156=VECTOR('',#7616,1.);
#2157=VECTOR('',#7617,1.);
#2158=VECTOR('',#7620,1.);
#2159=VECTOR('',#7621,1.);
#2160=CIRCLE('',#5436,0.275);
#2161=CIRCLE('',#5437,0.275);
#2162=CIRCLE('',#5439,0.275);
#2163=CIRCLE('',#5440,0.275);
#2164=CIRCLE('',#5442,0.275);
#2165=CIRCLE('',#5443,0.275);
#2166=CIRCLE('',#5445,0.275);
#2167=CIRCLE('',#5446,0.275);
#2168=CIRCLE('',#5448,0.275);
#2169=CIRCLE('',#5449,0.275);
#2170=CIRCLE('',#5451,0.275);
#2171=CIRCLE('',#5452,0.275);
#2172=CIRCLE('',#5454,0.275);
#2173=CIRCLE('',#5455,0.275);
#2174=CIRCLE('',#5457,0.275);
#2175=CIRCLE('',#5458,0.275);
#2176=CIRCLE('',#5460,0.275);
#2177=CIRCLE('',#5461,0.275);
#2178=CIRCLE('',#5484,0.165);
#2179=CIRCLE('',#5485,0.165);
#2180=CIRCLE('',#5488,0.165);
#2181=CIRCLE('',#5489,0.165);
#2182=CIRCLE('',#5492,0.165);
#2183=CIRCLE('',#5493,0.165);
#2184=CIRCLE('',#5496,0.165);
#2185=CIRCLE('',#5497,0.165);
#2186=CIRCLE('',#5500,0.21);
#2187=CIRCLE('',#5501,0.21);
#2188=CIRCLE('',#5504,0.21);
#2189=CIRCLE('',#5505,0.21);
#2190=CIRCLE('',#5508,0.21);
#2191=CIRCLE('',#5509,0.21);
#2192=CIRCLE('',#5512,0.21);
#2193=CIRCLE('',#5513,0.21);
#2194=CIRCLE('',#5516,1.05);
#2195=CIRCLE('',#5517,1.05);
#2196=CIRCLE('',#5519,0.625);
#2197=CIRCLE('',#5521,0.625);
#2198=CIRCLE('',#5530,0.375);
#2199=CIRCLE('',#5531,0.375);
#2200=CIRCLE('',#5533,0.225);
#2201=CIRCLE('',#5535,0.375);
#2202=CIRCLE('',#5536,0.375);
#2203=CIRCLE('',#5538,0.225);
#2204=CIRCLE('',#5540,0.375);
#2205=CIRCLE('',#5541,0.375);
#2206=CIRCLE('',#5543,0.225);
#2207=CIRCLE('',#5545,0.375);
#2208=CIRCLE('',#5546,0.375);
#2209=CIRCLE('',#5548,0.225);
#2210=CIRCLE('',#5550,0.225);
#2211=CIRCLE('',#5552,0.225);
#2212=CIRCLE('',#5554,0.225);
#2213=CIRCLE('',#5556,0.225);
#2214=CIRCLE('',#5558,1.04);
#2215=CIRCLE('',#5559,1.04);
#2216=CIRCLE('',#5561,0.625);
#2217=CIRCLE('',#5563,0.625);
#2218=CIRCLE('',#5565,2.);
#2219=CIRCLE('',#5566,2.);
#2220=CIRCLE('',#5571,0.625);
#2221=CIRCLE('',#5572,0.625);
#2222=CIRCLE('',#5574,0.8);
#2223=CIRCLE('',#5575,0.8);
#2224=CIRCLE('',#5579,0.06);
#2225=CIRCLE('',#5580,0.06);
#2226=CIRCLE('',#5585,0.21);
#2227=CIRCLE('',#5586,0.21);
#2228=CIRCLE('',#5599,0.8);
#2229=CIRCLE('',#5601,0.2);
#2230=CIRCLE('',#5603,0.2);
#2231=CIRCLE('',#5605,1.);
#2232=CIRCLE('',#5606,1.);
#2233=CIRCLE('',#5608,0.515);
#2234=CIRCLE('',#5609,0.515);
#2235=CIRCLE('',#5612,0.8);
#2236=CIRCLE('',#5615,2.4);
#2237=CIRCLE('',#5616,2.4);
#2238=CIRCLE('',#5617,2.4);
#2239=CIRCLE('',#5619,1.25);
#2240=CIRCLE('',#5620,1.25);
#2241=CIRCLE('',#5622,1.);
#2242=CIRCLE('',#5625,0.275);
#2243=CIRCLE('',#5626,0.275);
#2244=CIRCLE('',#5628,0.275);
#2245=CIRCLE('',#5629,0.275);
#2246=CIRCLE('',#5631,0.275);
#2247=CIRCLE('',#5632,0.275);
#2248=CIRCLE('',#5634,0.275);
#2249=CIRCLE('',#5635,0.275);
#2250=CIRCLE('',#5640,1.);
#2251=CIRCLE('',#5641,1.);
#2252=CIRCLE('',#5643,1.25);
#2253=CIRCLE('',#5644,1.25);
#2254=CIRCLE('',#5649,0.15);
#2255=CIRCLE('',#5651,0.15);
#2256=CIRCLE('',#5653,0.2);
#2257=CIRCLE('',#5654,0.2);
#2258=CIRCLE('',#5656,0.2);
#2259=CIRCLE('',#5658,0.515);
#2260=CIRCLE('',#5659,0.515);
#2261=CIRCLE('',#5662,0.8);
#2262=CIRCLE('',#5665,0.5);
#2263=CIRCLE('',#5666,0.5);
#2264=CIRCLE('',#5668,0.41);
#2265=CIRCLE('',#5670,0.41);
#2266=CIRCLE('',#5672,0.41);
#2267=CIRCLE('',#5674,0.41);
#2268=CIRCLE('',#5676,1.25);
#2269=CIRCLE('',#5677,1.25);
#2270=CIRCLE('',#5679,1.);
#2271=CIRCLE('',#5681,1.);
#2272=CIRCLE('',#5684,0.275);
#2273=CIRCLE('',#5685,0.275);
#2274=CIRCLE('',#5687,0.275);
#2275=CIRCLE('',#5688,0.275);
#2276=CIRCLE('',#5690,0.275);
#2277=CIRCLE('',#5691,0.275);
#2278=CIRCLE('',#5693,0.275);
#2279=CIRCLE('',#5694,0.275);
#2280=CIRCLE('',#5696,2.4);
#2281=CIRCLE('',#5697,2.4);
#2282=CIRCLE('',#5702,1.);
#2283=CIRCLE('',#5703,1.);
#2284=CIRCLE('',#5705,1.25);
#2285=CIRCLE('',#5706,1.25);
#2286=CIRCLE('',#5711,1.);
#2287=CIRCLE('',#5712,1.);
#2288=CIRCLE('',#5714,1.25);
#2289=CIRCLE('',#5715,1.25);
#2290=CIRCLE('',#5720,0.4);
#2291=CIRCLE('',#5721,0.4);
#2292=CIRCLE('',#5723,0.5);
#2293=CIRCLE('',#5724,0.5);
#2294=CIRCLE('',#5729,0.25);
#2295=CIRCLE('',#5730,0.25);
#2296=CIRCLE('',#5735,0.25);
#2297=CIRCLE('',#5736,0.25);
#2298=CIRCLE('',#5741,0.25);
#2299=CIRCLE('',#5742,0.25);
#2300=CIRCLE('',#5747,0.25);
#2301=CIRCLE('',#5748,0.25);
#2302=CIRCLE('',#5754,0.9);
#2303=CIRCLE('',#5757,0.9);
#2304=CIRCLE('',#5761,1.05);
#2305=CIRCLE('',#5762,0.9);
#2306=CIRCLE('',#5764,1.05);
#2307=CIRCLE('',#5766,1.);
#2308=CIRCLE('',#5768,1.);
#2309=CIRCLE('',#5770,1.05);
#2310=CIRCLE('',#5772,1.05);
#2311=CIRCLE('',#5774,1.);
#2312=CIRCLE('',#5776,1.);
#2313=CIRCLE('',#5778,1.05);
#2314=CIRCLE('',#5780,1.05);
#2315=CIRCLE('',#5782,0.9);
#2316=CIRCLE('',#5786,0.895);
#2317=CIRCLE('',#5787,0.605);
#2318=CIRCLE('',#5790,0.895);
#2319=CIRCLE('',#5791,0.605);
#2320=CIRCLE('',#5794,0.895);
#2321=CIRCLE('',#5795,0.605);
#2322=CIRCLE('',#5797,0.895);
#2323=CIRCLE('',#5799,0.605);
#2324=CIRCLE('',#5805,0.375);
#2325=CIRCLE('',#5807,0.425);
#2326=CIRCLE('',#5809,0.425);
#2327=CIRCLE('',#5811,0.395);
#2328=CIRCLE('',#5813,0.27);
#2329=CIRCLE('',#5815,0.24505);
#2330=CIRCLE('',#5817,0.24505);
#2331=CIRCLE('',#5819,0.2);
#2332=CIRCLE('',#5832,0.43);
#2333=CIRCLE('',#5833,0.43);
#2334=CIRCLE('',#5835,0.2);
#2335=CIRCLE('',#5837,0.525);
#2336=CIRCLE('',#5839,0.515);
#2337=CIRCLE('',#5847,0.46);
#2338=CIRCLE('',#5849,0.46);
#2339=CIRCLE('',#5851,0.525);
#2340=CIRCLE('',#5854,0.515);
#2341=CIRCLE('',#5856,0.2);
#2342=CIRCLE('',#5860,0.475);
#2343=CIRCLE('',#5861,0.31);
#2344=CIRCLE('',#5863,0.475);
#2345=CIRCLE('',#5865,0.355);
#2346=CIRCLE('',#5867,0.355);
#2347=CIRCLE('',#5869,0.31);
#2348=CIRCLE('',#5875,0.285);
#2349=CIRCLE('',#5876,0.265);
#2350=CIRCLE('',#5878,0.265);
#2351=CIRCLE('',#5880,0.5);
#2352=CIRCLE('',#5882,0.5);
#2353=CIRCLE('',#5886,0.38);
#2354=CIRCLE('',#5888,0.38);
#2355=CIRCLE('',#5893,0.2117);
#2356=CIRCLE('',#5894,0.2117);
#2357=CIRCLE('',#5903,0.4);
#2358=CIRCLE('',#5904,0.4);
#2359=CIRCLE('',#5906,0.225);
#2360=CIRCLE('',#5908,0.225);
#2361=CIRCLE('',#5917,0.164999999999999);
#2362=CIRCLE('',#5919,0.164999999999999);
#2363=CIRCLE('',#5922,0.605);
#2364=CIRCLE('',#5923,0.605);
#2365=CIRCLE('',#5924,0.605);
#2366=CIRCLE('',#5926,0.605);
#2367=CIRCLE('',#5927,0.605);
#2368=CIRCLE('',#5928,0.605);
#2369=CIRCLE('',#5931,1.);
#2370=CIRCLE('',#5933,1.);
#2371=CIRCLE('',#5935,1.);
#2372=CIRCLE('',#5936,1.);
#2373=CIRCLE('',#5937,1.);
#2374=CIRCLE('',#5938,1.);
#2375=CIRCLE('',#5946,0.165);
#2376=CIRCLE('',#5947,0.165);
#2377=CIRCLE('',#5950,0.165);
#2378=CIRCLE('',#5951,0.165);
#2379=CIRCLE('',#5954,0.4);
#2380=CIRCLE('',#5955,0.4);
#2381=CIRCLE('',#5960,0.94);
#2382=CIRCLE('',#5961,0.94);
#2383=CIRCLE('',#5963,0.99);
#2384=CIRCLE('',#5965,0.99);
#2385=CIRCLE('',#5967,0.99);
#2386=CIRCLE('',#5969,0.225);
#2387=CIRCLE('',#5970,0.225);
#2388=CIRCLE('',#5972,0.99);
#2389=CIRCLE('',#5977,0.94);
#2390=CIRCLE('',#5978,0.94);
#2391=CIRCLE('',#5980,1.);
#2392=CIRCLE('',#5981,1.);
#2393=CIRCLE('',#5986,0.6);
#2394=CIRCLE('',#5988,0.6);
#2395=CIRCLE('',#5989,0.5);
#2396=CIRCLE('',#5994,0.1954);
#2397=CIRCLE('',#6003,0.17);
#2398=CIRCLE('',#6005,0.1954);
#2399=CIRCLE('',#6009,0.3);
#2400=CIRCLE('',#6011,0.35);
#2401=CIRCLE('',#6013,0.35);
#2402=CIRCLE('',#6015,0.32);
#2403=CIRCLE('',#6017,0.22);
#2404=CIRCLE('',#6019,0.1954);
#2405=CIRCLE('',#6021,0.1954);
#2406=CIRCLE('',#6023,0.16);
#2407=VERTEX_POINT('',#7742);
#2408=VERTEX_POINT('',#7744);
#2409=VERTEX_POINT('',#7748);
#2410=VERTEX_POINT('',#7750);
#2411=VERTEX_POINT('',#7754);
#2412=VERTEX_POINT('',#7756);
#2413=VERTEX_POINT('',#7760);
#2414=VERTEX_POINT('',#7762);
#2415=VERTEX_POINT('',#7766);
#2416=VERTEX_POINT('',#7768);
#2417=VERTEX_POINT('',#7772);
#2418=VERTEX_POINT('',#7774);
#2419=VERTEX_POINT('',#7778);
#2420=VERTEX_POINT('',#7780);
#2421=VERTEX_POINT('',#7784);
#2422=VERTEX_POINT('',#7786);
#2423=VERTEX_POINT('',#7790);
#2424=VERTEX_POINT('',#7792);
#2425=VERTEX_POINT('',#7796);
#2426=VERTEX_POINT('',#7797);
#2427=VERTEX_POINT('',#7799);
#2428=VERTEX_POINT('',#7801);
#2429=VERTEX_POINT('',#7805);
#2430=VERTEX_POINT('',#7807);
#2431=VERTEX_POINT('',#7811);
#2432=VERTEX_POINT('',#7813);
#2433=VERTEX_POINT('',#7823);
#2434=VERTEX_POINT('',#7824);
#2435=VERTEX_POINT('',#7826);
#2436=VERTEX_POINT('',#7828);
#2437=VERTEX_POINT('',#7832);
#2438=VERTEX_POINT('',#7834);
#2439=VERTEX_POINT('',#7838);
#2440=VERTEX_POINT('',#7840);
#2441=VERTEX_POINT('',#7850);
#2442=VERTEX_POINT('',#7851);
#2443=VERTEX_POINT('',#7853);
#2444=VERTEX_POINT('',#7855);
#2445=VERTEX_POINT('',#7859);
#2446=VERTEX_POINT('',#7861);
#2447=VERTEX_POINT('',#7865);
#2448=VERTEX_POINT('',#7867);
#2449=VERTEX_POINT('',#7877);
#2450=VERTEX_POINT('',#7879);
#2451=VERTEX_POINT('',#7884);
#2452=VERTEX_POINT('',#7886);
#2453=VERTEX_POINT('',#7891);
#2454=VERTEX_POINT('',#7893);
#2455=VERTEX_POINT('',#7898);
#2456=VERTEX_POINT('',#7900);
#2457=VERTEX_POINT('',#7905);
#2458=VERTEX_POINT('',#7907);
#2459=VERTEX_POINT('',#7912);
#2460=VERTEX_POINT('',#7914);
#2461=VERTEX_POINT('',#7919);
#2462=VERTEX_POINT('',#7921);
#2463=VERTEX_POINT('',#7926);
#2464=VERTEX_POINT('',#7928);
#2465=VERTEX_POINT('',#7933);
#2466=VERTEX_POINT('',#7935);
#2467=VERTEX_POINT('',#7939);
#2468=VERTEX_POINT('',#7942);
#2469=VERTEX_POINT('',#7946);
#2470=VERTEX_POINT('',#7947);
#2471=VERTEX_POINT('',#7949);
#2472=VERTEX_POINT('',#7951);
#2473=VERTEX_POINT('',#7955);
#2474=VERTEX_POINT('',#7957);
#2475=VERTEX_POINT('',#7961);
#2476=VERTEX_POINT('',#7963);
#2477=VERTEX_POINT('',#7973);
#2478=VERTEX_POINT('',#7975);
#2479=VERTEX_POINT('',#7979);
#2480=VERTEX_POINT('',#7982);
#2481=VERTEX_POINT('',#7984);
#2482=VERTEX_POINT('',#7988);
#2483=VERTEX_POINT('',#7991);
#2484=VERTEX_POINT('',#7993);
#2485=VERTEX_POINT('',#7997);
#2486=VERTEX_POINT('',#8000);
#2487=VERTEX_POINT('',#8002);
#2488=VERTEX_POINT('',#8006);
#2489=VERTEX_POINT('',#8009);
#2490=VERTEX_POINT('',#8013);
#2491=VERTEX_POINT('',#8017);
#2492=VERTEX_POINT('',#8021);
#2493=VERTEX_POINT('',#8025);
#2494=VERTEX_POINT('',#8027);
#2495=VERTEX_POINT('',#8031);
#2496=VERTEX_POINT('',#8034);
#2497=VERTEX_POINT('',#8038);
#2498=VERTEX_POINT('',#8040);
#2499=VERTEX_POINT('',#8047);
#2500=VERTEX_POINT('',#8049);
#2501=VERTEX_POINT('',#8053);
#2502=VERTEX_POINT('',#8055);
#2503=VERTEX_POINT('',#8821);
#2504=VERTEX_POINT('',#8823);
#2505=VERTEX_POINT('',#8905);
#2506=VERTEX_POINT('',#8907);
#2507=VERTEX_POINT('',#8912);
#2508=VERTEX_POINT('',#8913);
#2509=VERTEX_POINT('',#8915);
#2510=VERTEX_POINT('',#8917);
#2511=VERTEX_POINT('',#8919);
#2512=VERTEX_POINT('',#8921);
#2513=VERTEX_POINT('',#8925);
#2514=VERTEX_POINT('',#8927);
#2515=VERTEX_POINT('',#8931);
#2516=VERTEX_POINT('',#8935);
#2517=VERTEX_POINT('',#8936);
#2518=VERTEX_POINT('',#8938);
#2519=VERTEX_POINT('',#8943);
#2520=VERTEX_POINT('',#8948);
#2521=VERTEX_POINT('',#8957);
#2522=VERTEX_POINT('',#8958);
#2523=VERTEX_POINT('',#8960);
#2524=VERTEX_POINT('',#8962);
#2525=VERTEX_POINT('',#8991);
#2526=VERTEX_POINT('',#8992);
#2527=VERTEX_POINT('',#8996);
#2528=VERTEX_POINT('',#8998);
#2529=VERTEX_POINT('',#9017);
#2530=VERTEX_POINT('',#9022);
#2531=VERTEX_POINT('',#9026);
#2532=VERTEX_POINT('',#9028);
#2533=VERTEX_POINT('',#9047);
#2534=VERTEX_POINT('',#9050);
#2535=VERTEX_POINT('',#9054);
#2536=VERTEX_POINT('',#9056);
#2537=VERTEX_POINT('',#9060);
#2538=VERTEX_POINT('',#9065);
#2539=VERTEX_POINT('',#9067);
#2540=VERTEX_POINT('',#9071);
#2541=VERTEX_POINT('',#9073);
#2542=VERTEX_POINT('',#9077);
#2543=VERTEX_POINT('',#9079);
#2544=VERTEX_POINT('',#9083);
#2545=VERTEX_POINT('',#9085);
#2546=VERTEX_POINT('',#9092);
#2547=VERTEX_POINT('',#9094);
#2548=VERTEX_POINT('',#9098);
#2549=VERTEX_POINT('',#9100);
#2550=VERTEX_POINT('',#9107);
#2551=VERTEX_POINT('',#9108);
#2552=VERTEX_POINT('',#9112);
#2553=VERTEX_POINT('',#9114);
#2554=VERTEX_POINT('',#9116);
#2555=VERTEX_POINT('',#9126);
#2556=VERTEX_POINT('',#9158);
#2557=VERTEX_POINT('',#9162);
#2558=VERTEX_POINT('',#9166);
#2559=VERTEX_POINT('',#9168);
#2560=VERTEX_POINT('',#9173);
#2561=VERTEX_POINT('',#9175);
#2562=VERTEX_POINT('',#9213);
#2563=VERTEX_POINT('',#9215);
#2564=VERTEX_POINT('',#9219);
#2565=VERTEX_POINT('',#9222);
#2566=VERTEX_POINT('',#9225);
#2567=VERTEX_POINT('',#9229);
#2568=VERTEX_POINT('',#9233);
#2569=VERTEX_POINT('',#9235);
#2570=VERTEX_POINT('',#9239);
#2571=VERTEX_POINT('',#9242);
#2572=VERTEX_POINT('',#9247);
#2573=VERTEX_POINT('',#9249);
#2574=VERTEX_POINT('',#9253);
#2575=VERTEX_POINT('',#9255);
#2576=VERTEX_POINT('',#9259);
#2577=VERTEX_POINT('',#9261);
#2578=VERTEX_POINT('',#9265);
#2579=VERTEX_POINT('',#9267);
#2580=VERTEX_POINT('',#9271);
#2581=VERTEX_POINT('',#9273);
#2582=VERTEX_POINT('',#9280);
#2583=VERTEX_POINT('',#9282);
#2584=VERTEX_POINT('',#9286);
#2585=VERTEX_POINT('',#9288);
#2586=VERTEX_POINT('',#9295);
#2587=VERTEX_POINT('',#9297);
#2588=VERTEX_POINT('',#9301);
#2589=VERTEX_POINT('',#9303);
#2590=VERTEX_POINT('',#9310);
#2591=VERTEX_POINT('',#9312);
#2592=VERTEX_POINT('',#9316);
#2593=VERTEX_POINT('',#9318);
#2594=VERTEX_POINT('',#9325);
#2595=VERTEX_POINT('',#9327);
#2596=VERTEX_POINT('',#9334);
#2597=VERTEX_POINT('',#9336);
#2598=VERTEX_POINT('',#9343);
#2599=VERTEX_POINT('',#9345);
#2600=VERTEX_POINT('',#9352);
#2601=VERTEX_POINT('',#9354);
#2602=VERTEX_POINT('',#9362);
#2603=VERTEX_POINT('',#9363);
#2604=VERTEX_POINT('',#9365);
#2605=VERTEX_POINT('',#9367);
#2606=VERTEX_POINT('',#9371);
#2607=VERTEX_POINT('',#9373);
#2608=VERTEX_POINT('',#9377);
#2609=VERTEX_POINT('',#9379);
#2610=VERTEX_POINT('',#9387);
#2611=VERTEX_POINT('',#9389);
#2612=VERTEX_POINT('',#9392);
#2613=VERTEX_POINT('',#9396);
#2614=VERTEX_POINT('',#9399);
#2615=VERTEX_POINT('',#9403);
#2616=VERTEX_POINT('',#9406);
#2617=VERTEX_POINT('',#9410);
#2618=VERTEX_POINT('',#9413);
#2619=VERTEX_POINT('',#9417);
#2620=VERTEX_POINT('',#9420);
#2621=VERTEX_POINT('',#9424);
#2622=VERTEX_POINT('',#9430);
#2623=VERTEX_POINT('',#9431);
#2624=VERTEX_POINT('',#9433);
#2625=VERTEX_POINT('',#9435);
#2626=VERTEX_POINT('',#9439);
#2627=VERTEX_POINT('',#9441);
#2628=VERTEX_POINT('',#9445);
#2629=VERTEX_POINT('',#9447);
#2630=VERTEX_POINT('',#9454);
#2631=VERTEX_POINT('',#9456);
#2632=VERTEX_POINT('',#9459);
#2633=VERTEX_POINT('',#9463);
#2634=VERTEX_POINT('',#9471);
#2635=VERTEX_POINT('',#9474);
#2636=VERTEX_POINT('',#9478);
#2637=VERTEX_POINT('',#9482);
#2638=VERTEX_POINT('',#9486);
#2639=VERTEX_POINT('',#9489);
#2640=VERTEX_POINT('',#9493);
#2641=VERTEX_POINT('',#9497);
#2642=VERTEX_POINT('',#9502);
#2643=VERTEX_POINT('',#9503);
#2644=VERTEX_POINT('',#9505);
#2645=VERTEX_POINT('',#9507);
#2646=VERTEX_POINT('',#9511);
#2647=VERTEX_POINT('',#9513);
#2648=VERTEX_POINT('',#9517);
#2649=VERTEX_POINT('',#9519);
#2650=VERTEX_POINT('',#9523);
#2651=VERTEX_POINT('',#9525);
#2652=VERTEX_POINT('',#9529);
#2653=VERTEX_POINT('',#9531);
#2654=VERTEX_POINT('',#9542);
#2655=VERTEX_POINT('',#9544);
#2656=VERTEX_POINT('',#9548);
#2657=VERTEX_POINT('',#9551);
#2658=VERTEX_POINT('',#9552);
#2659=VERTEX_POINT('',#9554);
#2660=VERTEX_POINT('',#9556);
#2661=VERTEX_POINT('',#9558);
#2662=VERTEX_POINT('',#9560);
#2663=VERTEX_POINT('',#9563);
#2664=VERTEX_POINT('',#9566);
#2665=VERTEX_POINT('',#9567);
#2666=VERTEX_POINT('',#9569);
#2667=VERTEX_POINT('',#9571);
#2668=VERTEX_POINT('',#9573);
#2669=VERTEX_POINT('',#9575);
#2670=VERTEX_POINT('',#9578);
#2671=VERTEX_POINT('',#9593);
#2672=VERTEX_POINT('',#9596);
#2673=VERTEX_POINT('',#9600);
#2674=VERTEX_POINT('',#9605);
#2675=VERTEX_POINT('',#9609);
#2676=VERTEX_POINT('',#9615);
#2677=VERTEX_POINT('',#9617);
#2678=VERTEX_POINT('',#9620);
#2679=VERTEX_POINT('',#9624);
#2680=VERTEX_POINT('',#9627);
#2681=VERTEX_POINT('',#9631);
#2682=VERTEX_POINT('',#9639);
#2683=VERTEX_POINT('',#9641);
#2684=VERTEX_POINT('',#9645);
#2685=VERTEX_POINT('',#9649);
#2686=VERTEX_POINT('',#9652);
#2687=VERTEX_POINT('',#9658);
#2688=VERTEX_POINT('',#9659);
#2689=VERTEX_POINT('',#9663);
#2690=VERTEX_POINT('',#9667);
#2691=VERTEX_POINT('',#9670);
#2692=VERTEX_POINT('',#9674);
#2693=VERTEX_POINT('',#9678);
#2694=VERTEX_POINT('',#9686);
#2695=VERTEX_POINT('',#9688);
#2696=VERTEX_POINT('',#9690);
#2697=VERTEX_POINT('',#9694);
#2698=VERTEX_POINT('',#9698);
#2699=VERTEX_POINT('',#9702);
#2700=VERTEX_POINT('',#9706);
#2701=VERTEX_POINT('',#9721);
#2702=VERTEX_POINT('',#9723);
#2703=VERTEX_POINT('',#9736);
#2704=VERTEX_POINT('',#9738);
#2705=VERTEX_POINT('',#9742);
#2706=VERTEX_POINT('',#9745);
#2707=VERTEX_POINT('',#9749);
#2708=VERTEX_POINT('',#9750);
#2709=VERTEX_POINT('',#9752);
#2710=VERTEX_POINT('',#9754);
#2711=VERTEX_POINT('',#9758);
#2712=VERTEX_POINT('',#9760);
#2713=VERTEX_POINT('',#9764);
#2714=VERTEX_POINT('',#9766);
#2715=VERTEX_POINT('',#9770);
#2716=VERTEX_POINT('',#9771);
#2717=VERTEX_POINT('',#9776);
#2718=VERTEX_POINT('',#9780);
#2719=VERTEX_POINT('',#9782);
#2720=VERTEX_POINT('',#9784);
#2721=VERTEX_POINT('',#9788);
#2722=VERTEX_POINT('',#9790);
#2723=VERTEX_POINT('',#9792);
#2724=VERTEX_POINT('',#9794);
#2725=VERTEX_POINT('',#9796);
#2726=VERTEX_POINT('',#9798);
#2727=VERTEX_POINT('',#9800);
#2728=VERTEX_POINT('',#9802);
#2729=VERTEX_POINT('',#9806);
#2730=VERTEX_POINT('',#9807);
#2731=VERTEX_POINT('',#9811);
#2732=VERTEX_POINT('',#9826);
#2733=VERTEX_POINT('',#9828);
#2734=VERTEX_POINT('',#9837);
#2735=VERTEX_POINT('',#9839);
#2736=VERTEX_POINT('',#9887);
#2737=VERTEX_POINT('',#9889);
#2738=VERTEX_POINT('',#9891);
#2739=VERTEX_POINT('',#9895);
#2740=VERTEX_POINT('',#9898);
#2741=VERTEX_POINT('',#9900);
#2742=VERTEX_POINT('',#9905);
#2743=VERTEX_POINT('',#9908);
#2744=VERTEX_POINT('',#9910);
#2745=VERTEX_POINT('',#9912);
#2746=VERTEX_POINT('',#9920);
#2747=VERTEX_POINT('',#9924);
#2748=VERTEX_POINT('',#9936);
#2749=VERTEX_POINT('',#9938);
#2750=VERTEX_POINT('',#9943);
#2751=VERTEX_POINT('',#9945);
#2752=VERTEX_POINT('',#9950);
#2753=VERTEX_POINT('',#9952);
#2754=VERTEX_POINT('',#9959);
#2755=VERTEX_POINT('',#9961);
#2756=VERTEX_POINT('',#9965);
#2757=VERTEX_POINT('',#9968);
#2758=VERTEX_POINT('',#9971);
#2759=VERTEX_POINT('',#9975);
#2760=VERTEX_POINT('',#9977);
#2761=VERTEX_POINT('',#9981);
#2762=VERTEX_POINT('',#9988);
#2763=VERTEX_POINT('',#9990);
#2764=VERTEX_POINT('',#9994);
#2765=VERTEX_POINT('',#9996);
#2766=VERTEX_POINT('',#10003);
#2767=VERTEX_POINT('',#10006);
#2768=VERTEX_POINT('',#10008);
#2769=VERTEX_POINT('',#10016);
#2770=VERTEX_POINT('',#10019);
#2771=VERTEX_POINT('',#10020);
#2772=VERTEX_POINT('',#10022);
#2773=VERTEX_POINT('',#10024);
#2774=VERTEX_POINT('',#10028);
#2775=VERTEX_POINT('',#10030);
#2776=VERTEX_POINT('',#10034);
#2777=VERTEX_POINT('',#10036);
#2778=VERTEX_POINT('',#10040);
#2779=VERTEX_POINT('',#10042);
#2780=VERTEX_POINT('',#10046);
#2781=VERTEX_POINT('',#10048);
#2782=VERTEX_POINT('',#10056);
#2783=VERTEX_POINT('',#10059);
#2784=VERTEX_POINT('',#10066);
#2785=VERTEX_POINT('',#10069);
#2786=VERTEX_POINT('',#10073);
#2787=VERTEX_POINT('',#10077);
#2788=VERTEX_POINT('',#10081);
#2789=VERTEX_POINT('',#10084);
#2790=VERTEX_POINT('',#10088);
#2791=VERTEX_POINT('',#10092);
#2792=VERTEX_POINT('',#10097);
#2793=VERTEX_POINT('',#10098);
#2794=VERTEX_POINT('',#10100);
#2795=VERTEX_POINT('',#10102);
#2796=VERTEX_POINT('',#10106);
#2797=VERTEX_POINT('',#10108);
#2798=VERTEX_POINT('',#10112);
#2799=VERTEX_POINT('',#10114);
#2800=VERTEX_POINT('',#10118);
#2801=VERTEX_POINT('',#10120);
#2802=VERTEX_POINT('',#10124);
#2803=VERTEX_POINT('',#10126);
#2804=EDGE_CURVE('',#2407,#2407,#2160,.T.);
#2805=EDGE_CURVE('',#2407,#2408,#1490,.T.);
#2806=EDGE_CURVE('',#2408,#2408,#2161,.T.);
#2807=EDGE_CURVE('',#2409,#2409,#2162,.T.);
#2808=EDGE_CURVE('',#2409,#2410,#1491,.T.);
#2809=EDGE_CURVE('',#2410,#2410,#2163,.T.);
#2810=EDGE_CURVE('',#2411,#2411,#2164,.T.);
#2811=EDGE_CURVE('',#2411,#2412,#1492,.T.);
#2812=EDGE_CURVE('',#2412,#2412,#2165,.T.);
#2813=EDGE_CURVE('',#2413,#2413,#2166,.T.);
#2814=EDGE_CURVE('',#2413,#2414,#1493,.T.);
#2815=EDGE_CURVE('',#2414,#2414,#2167,.T.);
#2816=EDGE_CURVE('',#2415,#2415,#2168,.T.);
#2817=EDGE_CURVE('',#2415,#2416,#1494,.T.);
#2818=EDGE_CURVE('',#2416,#2416,#2169,.T.);
#2819=EDGE_CURVE('',#2417,#2417,#2170,.T.);
#2820=EDGE_CURVE('',#2417,#2418,#1495,.T.);
#2821=EDGE_CURVE('',#2418,#2418,#2171,.T.);
#2822=EDGE_CURVE('',#2419,#2419,#2172,.T.);
#2823=EDGE_CURVE('',#2419,#2420,#1496,.T.);
#2824=EDGE_CURVE('',#2420,#2420,#2173,.T.);
#2825=EDGE_CURVE('',#2421,#2421,#2174,.T.);
#2826=EDGE_CURVE('',#2421,#2422,#1497,.T.);
#2827=EDGE_CURVE('',#2422,#2422,#2175,.T.);
#2828=EDGE_CURVE('',#2423,#2423,#2176,.T.);
#2829=EDGE_CURVE('',#2423,#2424,#1498,.T.);
#2830=EDGE_CURVE('',#2424,#2424,#2177,.T.);
#2831=EDGE_CURVE('',#2425,#2426,#1499,.T.);
#2832=EDGE_CURVE('',#2426,#2427,#1500,.T.);
#2833=EDGE_CURVE('',#2428,#2427,#1501,.T.);
#2834=EDGE_CURVE('',#2425,#2428,#1502,.T.);
#2835=EDGE_CURVE('',#2429,#2425,#1503,.T.);
#2836=EDGE_CURVE('',#2430,#2428,#1504,.T.);
#2837=EDGE_CURVE('',#2429,#2430,#1505,.T.);
#2838=EDGE_CURVE('',#2431,#2429,#1506,.T.);
#2839=EDGE_CURVE('',#2432,#2430,#1507,.T.);
#2840=EDGE_CURVE('',#2431,#2432,#1508,.T.);
#2841=EDGE_CURVE('',#2426,#2431,#1509,.T.);
#2842=EDGE_CURVE('',#2427,#2432,#1510,.T.);
#2843=EDGE_CURVE('',#2433,#2434,#1511,.T.);
#2844=EDGE_CURVE('',#2434,#2435,#1512,.T.);
#2845=EDGE_CURVE('',#2436,#2435,#1513,.T.);
#2846=EDGE_CURVE('',#2433,#2436,#1514,.T.);
#2847=EDGE_CURVE('',#2437,#2433,#1515,.T.);
#2848=EDGE_CURVE('',#2438,#2436,#1516,.T.);
#2849=EDGE_CURVE('',#2437,#2438,#1517,.T.);
#2850=EDGE_CURVE('',#2439,#2437,#1518,.T.);
#2851=EDGE_CURVE('',#2440,#2438,#1519,.T.);
#2852=EDGE_CURVE('',#2439,#2440,#1520,.T.);
#2853=EDGE_CURVE('',#2434,#2439,#1521,.T.);
#2854=EDGE_CURVE('',#2435,#2440,#1522,.T.);
#2855=EDGE_CURVE('',#2441,#2442,#1523,.T.);
#2856=EDGE_CURVE('',#2442,#2443,#1524,.T.);
#2857=EDGE_CURVE('',#2444,#2443,#1525,.T.);
#2858=EDGE_CURVE('',#2441,#2444,#1526,.T.);
#2859=EDGE_CURVE('',#2445,#2441,#1527,.T.);
#2860=EDGE_CURVE('',#2446,#2444,#1528,.T.);
#2861=EDGE_CURVE('',#2445,#2446,#1529,.T.);
#2862=EDGE_CURVE('',#2447,#2445,#1530,.T.);
#2863=EDGE_CURVE('',#2448,#2446,#1531,.T.);
#2864=EDGE_CURVE('',#2447,#2448,#1532,.T.);
#2865=EDGE_CURVE('',#2442,#2447,#1533,.T.);
#2866=EDGE_CURVE('',#2443,#2448,#1534,.T.);
#2867=EDGE_CURVE('',#2449,#2449,#2178,.T.);
#2868=EDGE_CURVE('',#2449,#2450,#1535,.T.);
#2869=EDGE_CURVE('',#2450,#2450,#2179,.T.);
#2870=EDGE_CURVE('',#2451,#2451,#2180,.T.);
#2871=EDGE_CURVE('',#2451,#2452,#1536,.T.);
#2872=EDGE_CURVE('',#2452,#2452,#2181,.T.);
#2873=EDGE_CURVE('',#2453,#2453,#2182,.T.);
#2874=EDGE_CURVE('',#2453,#2454,#1537,.T.);
#2875=EDGE_CURVE('',#2454,#2454,#2183,.T.);
#2876=EDGE_CURVE('',#2455,#2455,#2184,.T.);
#2877=EDGE_CURVE('',#2455,#2456,#1538,.T.);
#2878=EDGE_CURVE('',#2456,#2456,#2185,.T.);
#2879=EDGE_CURVE('',#2457,#2457,#2186,.T.);
#2880=EDGE_CURVE('',#2457,#2458,#1539,.T.);
#2881=EDGE_CURVE('',#2458,#2458,#2187,.T.);
#2882=EDGE_CURVE('',#2459,#2459,#2188,.T.);
#2883=EDGE_CURVE('',#2459,#2460,#1540,.T.);
#2884=EDGE_CURVE('',#2460,#2460,#2189,.T.);
#2885=EDGE_CURVE('',#2461,#2461,#2190,.T.);
#2886=EDGE_CURVE('',#2461,#2462,#1541,.T.);
#2887=EDGE_CURVE('',#2462,#2462,#2191,.T.);
#2888=EDGE_CURVE('',#2463,#2463,#2192,.T.);
#2889=EDGE_CURVE('',#2463,#2464,#1542,.T.);
#2890=EDGE_CURVE('',#2464,#2464,#2193,.T.);
#2891=EDGE_CURVE('',#2465,#2465,#2194,.T.);
#2892=EDGE_CURVE('',#2465,#2466,#1543,.T.);
#2893=EDGE_CURVE('',#2466,#2466,#2195,.T.);
#2894=EDGE_CURVE('',#2467,#2467,#2196,.T.);
#2895=EDGE_CURVE('',#2468,#2468,#2197,.T.);
#2896=EDGE_CURVE('',#2468,#2467,#1544,.T.);
#2897=EDGE_CURVE('',#2469,#2470,#1545,.T.);
#2898=EDGE_CURVE('',#2470,#2471,#1546,.T.);
#2899=EDGE_CURVE('',#2472,#2471,#1547,.T.);
#2900=EDGE_CURVE('',#2469,#2472,#1548,.T.);
#2901=EDGE_CURVE('',#2473,#2469,#1549,.T.);
#2902=EDGE_CURVE('',#2474,#2472,#1550,.T.);
#2903=EDGE_CURVE('',#2473,#2474,#1551,.T.);
#2904=EDGE_CURVE('',#2475,#2473,#1552,.T.);
#2905=EDGE_CURVE('',#2476,#2474,#1553,.T.);
#2906=EDGE_CURVE('',#2475,#2476,#1554,.T.);
#2907=EDGE_CURVE('',#2470,#2475,#1555,.T.);
#2908=EDGE_CURVE('',#2471,#2476,#1556,.T.);
#2909=EDGE_CURVE('',#2477,#2477,#2198,.T.);
#2910=EDGE_CURVE('',#2477,#2478,#1557,.T.);
#2911=EDGE_CURVE('',#2478,#2478,#2199,.T.);
#2912=EDGE_CURVE('',#2479,#2479,#2200,.T.);
#2913=EDGE_CURVE('',#2480,#2480,#2201,.T.);
#2914=EDGE_CURVE('',#2480,#2481,#1558,.T.);
#2915=EDGE_CURVE('',#2481,#2481,#2202,.T.);
#2916=EDGE_CURVE('',#2482,#2482,#2203,.T.);
#2917=EDGE_CURVE('',#2483,#2483,#2204,.T.);
#2918=EDGE_CURVE('',#2483,#2484,#1559,.T.);
#2919=EDGE_CURVE('',#2484,#2484,#2205,.T.);
#2920=EDGE_CURVE('',#2485,#2485,#2206,.T.);
#2921=EDGE_CURVE('',#2486,#2486,#2207,.T.);
#2922=EDGE_CURVE('',#2486,#2487,#1560,.T.);
#2923=EDGE_CURVE('',#2487,#2487,#2208,.T.);
#2924=EDGE_CURVE('',#2488,#2488,#2209,.T.);
#2925=EDGE_CURVE('',#2489,#2489,#2210,.T.);
#2926=EDGE_CURVE('',#2489,#2479,#1561,.T.);
#2927=EDGE_CURVE('',#2490,#2490,#2211,.T.);
#2928=EDGE_CURVE('',#2490,#2482,#1562,.T.);
#2929=EDGE_CURVE('',#2491,#2491,#2212,.T.);
#2930=EDGE_CURVE('',#2491,#2485,#1563,.T.);
#2931=EDGE_CURVE('',#2492,#2492,#2213,.T.);
#2932=EDGE_CURVE('',#2492,#2488,#1564,.T.);
#2933=EDGE_CURVE('',#2493,#2493,#2214,.T.);
#2934=EDGE_CURVE('',#2493,#2494,#1565,.T.);
#2935=EDGE_CURVE('',#2494,#2494,#2215,.T.);
#2936=EDGE_CURVE('',#2495,#2495,#2216,.T.);
#2937=EDGE_CURVE('',#2496,#2496,#2217,.T.);
#2938=EDGE_CURVE('',#2496,#2495,#1566,.T.);
#2939=EDGE_CURVE('',#2497,#2497,#2218,.T.);
#2940=EDGE_CURVE('',#2497,#2498,#1567,.T.);
#2941=EDGE_CURVE('',#2498,#2498,#2219,.T.);
#2942=EDGE_CURVE('',#2499,#2499,#2220,.T.);
#2943=EDGE_CURVE('',#2499,#2500,#1568,.T.);
#2944=EDGE_CURVE('',#2500,#2500,#2221,.T.);
#2945=EDGE_CURVE('',#2501,#2501,#2222,.T.);
#2946=EDGE_CURVE('',#2501,#2502,#1569,.T.);
#2947=EDGE_CURVE('',#2502,#2502,#2223,.T.);
#2948=EDGE_CURVE('',#2503,#2503,#2224,.T.);
#2949=EDGE_CURVE('',#2503,#2504,#280,.T.);
#2950=EDGE_CURVE('',#2504,#2504,#2225,.T.);
#2951=EDGE_CURVE('',#2505,#2505,#2226,.T.);
#2952=EDGE_CURVE('',#2505,#2506,#1570,.T.);
#2953=EDGE_CURVE('',#2506,#2506,#2227,.T.);
#2954=EDGE_CURVE('',#2507,#2508,#1571,.T.);
#2955=EDGE_CURVE('',#2509,#2507,#1572,.T.);
#2956=EDGE_CURVE('',#2510,#2509,#1573,.T.);
#2957=EDGE_CURVE('',#2511,#2510,#1574,.T.);
#2958=EDGE_CURVE('',#2512,#2511,#1575,.T.);
#2959=EDGE_CURVE('',#2508,#2512,#1576,.T.);
#2960=EDGE_CURVE('',#2510,#2513,#1577,.T.);
#2961=EDGE_CURVE('',#2514,#2513,#1578,.T.);
#2962=EDGE_CURVE('',#2511,#2514,#1579,.T.);
#2963=EDGE_CURVE('',#2515,#2514,#1580,.T.);
#2964=EDGE_CURVE('',#2512,#2515,#1581,.T.);
#2965=EDGE_CURVE('',#2516,#2517,#1582,.T.);
#2966=EDGE_CURVE('',#2516,#2518,#1583,.T.);
#2967=EDGE_CURVE('',#2518,#2508,#1584,.T.);
#2968=EDGE_CURVE('',#2517,#2515,#1585,.T.);
#2969=EDGE_CURVE('',#2519,#2509,#1586,.T.);
#2970=EDGE_CURVE('',#2519,#2516,#1587,.T.);
#2971=EDGE_CURVE('',#2513,#2517,#1588,.T.);
#2972=EDGE_CURVE('',#2520,#2507,#1589,.T.);
#2973=EDGE_CURVE('',#2520,#2519,#1590,.T.);
#2974=EDGE_CURVE('',#2518,#2520,#1591,.T.);
#2975=EDGE_CURVE('',#2521,#2522,#1592,.T.);
#2976=EDGE_CURVE('',#2523,#2521,#2228,.T.);
#2977=EDGE_CURVE('',#2523,#2524,#1593,.T.);
#2978=EDGE_CURVE('',#2522,#2524,#281,.T.);
#2979=EDGE_CURVE('',#2525,#2526,#1594,.T.);
#2980=EDGE_CURVE('',#2525,#2526,#2229,.T.);
#2981=EDGE_CURVE('',#2527,#2525,#1595,.T.);
#2982=EDGE_CURVE('',#2528,#2527,#282,.T.);
#2983=EDGE_CURVE('',#2528,#2529,#1596,.T.);
#2984=EDGE_CURVE('',#2529,#2529,#2230,.T.);
#2985=EDGE_CURVE('',#2526,#2528,#1597,.T.);
#2986=EDGE_CURVE('',#2528,#2530,#2231,.T.);
#2987=EDGE_CURVE('',#2530,#2527,#2232,.T.);
#2988=EDGE_CURVE('',#2531,#2531,#2233,.T.);
#2989=EDGE_CURVE('',#2531,#2532,#1598,.T.);
#2990=EDGE_CURVE('',#2532,#2532,#2234,.T.);
#2991=EDGE_CURVE('',#2524,#2522,#283,.T.);
#2992=EDGE_CURVE('',#2523,#2524,#1599,.T.);
#2993=EDGE_CURVE('',#2521,#2523,#2235,.T.);
#2994=EDGE_CURVE('',#2524,#2533,#2236,.T.);
#2995=EDGE_CURVE('',#2533,#2524,#2237,.T.);
#2996=EDGE_CURVE('',#2533,#2534,#1600,.T.);
#2997=EDGE_CURVE('',#2534,#2534,#2238,.T.);
#2998=EDGE_CURVE('',#2535,#2535,#2239,.T.);
#2999=EDGE_CURVE('',#2535,#2536,#1601,.T.);
#3000=EDGE_CURVE('',#2536,#2536,#2240,.T.);
#3001=EDGE_CURVE('',#2537,#2537,#2241,.T.);
#3002=EDGE_CURVE('',#2530,#2537,#1602,.T.);
#3003=EDGE_CURVE('',#2538,#2538,#2242,.T.);
#3004=EDGE_CURVE('',#2538,#2539,#1603,.T.);
#3005=EDGE_CURVE('',#2539,#2539,#2243,.T.);
#3006=EDGE_CURVE('',#2540,#2540,#2244,.T.);
#3007=EDGE_CURVE('',#2540,#2541,#1604,.T.);
#3008=EDGE_CURVE('',#2541,#2541,#2245,.T.);
#3009=EDGE_CURVE('',#2542,#2542,#2246,.T.);
#3010=EDGE_CURVE('',#2542,#2543,#1605,.T.);
#3011=EDGE_CURVE('',#2543,#2543,#2247,.T.);
#3012=EDGE_CURVE('',#2544,#2544,#2248,.T.);
#3013=EDGE_CURVE('',#2544,#2545,#1606,.T.);
#3014=EDGE_CURVE('',#2545,#2545,#2249,.T.);
#3015=EDGE_CURVE('',#2546,#2546,#2250,.T.);
#3016=EDGE_CURVE('',#2546,#2547,#1607,.T.);
#3017=EDGE_CURVE('',#2547,#2547,#2251,.T.);
#3018=EDGE_CURVE('',#2548,#2548,#2252,.T.);
#3019=EDGE_CURVE('',#2548,#2549,#1608,.T.);
#3020=EDGE_CURVE('',#2549,#2549,#2253,.T.);
#3021=EDGE_CURVE('',#2550,#2551,#1609,.T.);
#3022=EDGE_CURVE('',#2551,#2550,#2254,.T.);
#3023=EDGE_CURVE('',#2552,#2552,#2255,.T.);
#3024=EDGE_CURVE('',#2552,#2553,#1610,.T.);
#3025=EDGE_CURVE('',#2554,#2553,#284,.T.);
#3026=EDGE_CURVE('',#2551,#2554,#1611,.T.);
#3027=EDGE_CURVE('',#2555,#2550,#1612,.T.);
#3028=EDGE_CURVE('',#2553,#2555,#285,.T.);
#3029=EDGE_CURVE('',#2554,#2556,#2256,.T.);
#3030=EDGE_CURVE('',#2556,#2555,#2257,.T.);
#3031=EDGE_CURVE('',#2556,#2557,#1613,.T.);
#3032=EDGE_CURVE('',#2557,#2557,#2258,.T.);
#3033=EDGE_CURVE('',#2558,#2558,#2259,.T.);
#3034=EDGE_CURVE('',#2558,#2559,#1614,.T.);
#3035=EDGE_CURVE('',#2559,#2559,#2260,.T.);
#3036=EDGE_CURVE('',#2560,#2560,#2261,.T.);
#3037=EDGE_CURVE('',#2560,#2561,#1615,.T.);
#3038=EDGE_CURVE('',#2561,#2561,#286,.T.);
#3039=EDGE_CURVE('',#2562,#2562,#2262,.T.);
#3040=EDGE_CURVE('',#2562,#2563,#1616,.T.);
#3041=EDGE_CURVE('',#2563,#2563,#2263,.T.);
#3042=EDGE_CURVE('',#2564,#2564,#2264,.T.);
#3043=EDGE_CURVE('',#2565,#2565,#2265,.T.);
#3044=EDGE_CURVE('',#2566,#2566,#2266,.T.);
#3045=EDGE_CURVE('',#2566,#2565,#1617,.T.);
#3046=EDGE_CURVE('',#2564,#2567,#1618,.T.);
#3047=EDGE_CURVE('',#2567,#2567,#2267,.T.);
#3048=EDGE_CURVE('',#2568,#2568,#2268,.T.);
#3049=EDGE_CURVE('',#2568,#2569,#1619,.T.);
#3050=EDGE_CURVE('',#2569,#2569,#2269,.T.);
#3051=EDGE_CURVE('',#2570,#2570,#2270,.T.);
#3052=EDGE_CURVE('',#2570,#2571,#1620,.T.);
#3053=EDGE_CURVE('',#2571,#2571,#2271,.T.);
#3054=EDGE_CURVE('',#2572,#2572,#2272,.T.);
#3055=EDGE_CURVE('',#2572,#2573,#1621,.T.);
#3056=EDGE_CURVE('',#2573,#2573,#2273,.T.);
#3057=EDGE_CURVE('',#2574,#2574,#2274,.T.);
#3058=EDGE_CURVE('',#2574,#2575,#1622,.T.);
#3059=EDGE_CURVE('',#2575,#2575,#2275,.T.);
#3060=EDGE_CURVE('',#2576,#2576,#2276,.T.);
#3061=EDGE_CURVE('',#2576,#2577,#1623,.T.);
#3062=EDGE_CURVE('',#2577,#2577,#2277,.T.);
#3063=EDGE_CURVE('',#2578,#2578,#2278,.T.);
#3064=EDGE_CURVE('',#2578,#2579,#1624,.T.);
#3065=EDGE_CURVE('',#2579,#2579,#2279,.T.);
#3066=EDGE_CURVE('',#2580,#2580,#2280,.T.);
#3067=EDGE_CURVE('',#2580,#2581,#1625,.T.);
#3068=EDGE_CURVE('',#2581,#2581,#2281,.T.);
#3069=EDGE_CURVE('',#2582,#2582,#2282,.T.);
#3070=EDGE_CURVE('',#2582,#2583,#1626,.T.);
#3071=EDGE_CURVE('',#2583,#2583,#2283,.T.);
#3072=EDGE_CURVE('',#2584,#2584,#2284,.T.);
#3073=EDGE_CURVE('',#2584,#2585,#1627,.T.);
#3074=EDGE_CURVE('',#2585,#2585,#2285,.T.);
#3075=EDGE_CURVE('',#2586,#2586,#2286,.T.);
#3076=EDGE_CURVE('',#2586,#2587,#1628,.T.);
#3077=EDGE_CURVE('',#2587,#2587,#2287,.T.);
#3078=EDGE_CURVE('',#2588,#2588,#2288,.T.);
#3079=EDGE_CURVE('',#2588,#2589,#1629,.T.);
#3080=EDGE_CURVE('',#2589,#2589,#2289,.T.);
#3081=EDGE_CURVE('',#2590,#2590,#2290,.T.);
#3082=EDGE_CURVE('',#2590,#2591,#1630,.T.);
#3083=EDGE_CURVE('',#2591,#2591,#2291,.T.);
#3084=EDGE_CURVE('',#2592,#2592,#2292,.T.);
#3085=EDGE_CURVE('',#2592,#2593,#1631,.T.);
#3086=EDGE_CURVE('',#2593,#2593,#2293,.T.);
#3087=EDGE_CURVE('',#2594,#2594,#2294,.T.);
#3088=EDGE_CURVE('',#2594,#2595,#1632,.T.);
#3089=EDGE_CURVE('',#2595,#2595,#2295,.T.);
#3090=EDGE_CURVE('',#2596,#2596,#2296,.T.);
#3091=EDGE_CURVE('',#2596,#2597,#1633,.T.);
#3092=EDGE_CURVE('',#2597,#2597,#2297,.T.);
#3093=EDGE_CURVE('',#2598,#2598,#2298,.T.);
#3094=EDGE_CURVE('',#2598,#2599,#1634,.T.);
#3095=EDGE_CURVE('',#2599,#2599,#2299,.T.);
#3096=EDGE_CURVE('',#2600,#2600,#2300,.T.);
#3097=EDGE_CURVE('',#2600,#2601,#1635,.T.);
#3098=EDGE_CURVE('',#2601,#2601,#2301,.T.);
#3099=EDGE_CURVE('',#2602,#2603,#2302,.T.);
#3100=EDGE_CURVE('',#2604,#2602,#1636,.T.);
#3101=EDGE_CURVE('',#2605,#2604,#1637,.T.);
#3102=EDGE_CURVE('',#2603,#2605,#1638,.T.);
#3103=EDGE_CURVE('',#2603,#2606,#1639,.T.);
#3104=EDGE_CURVE('',#2607,#2605,#1640,.T.);
#3105=EDGE_CURVE('',#2607,#2606,#1641,.T.);
#3106=EDGE_CURVE('',#2606,#2608,#2303,.T.);
#3107=EDGE_CURVE('',#2609,#2607,#1642,.T.);
#3108=EDGE_CURVE('',#2608,#2609,#1643,.T.);
#3109=EDGE_CURVE('',#2608,#2602,#1644,.T.);
#3110=EDGE_CURVE('',#2609,#2604,#1645,.T.);
#3111=EDGE_CURVE('',#2610,#2610,#2304,.T.);
#3112=EDGE_CURVE('',#2611,#2611,#2305,.T.);
#3113=EDGE_CURVE('',#2612,#2612,#2306,.T.);
#3114=EDGE_CURVE('',#2612,#2610,#1646,.T.);
#3115=EDGE_CURVE('',#2613,#2613,#2307,.T.);
#3116=EDGE_CURVE('',#2614,#2614,#2308,.T.);
#3117=EDGE_CURVE('',#2614,#2613,#1647,.T.);
#3118=EDGE_CURVE('',#2615,#2615,#2309,.T.);
#3119=EDGE_CURVE('',#2616,#2616,#2310,.T.);
#3120=EDGE_CURVE('',#2616,#2615,#1648,.T.);
#3121=EDGE_CURVE('',#2617,#2617,#2311,.T.);
#3122=EDGE_CURVE('',#2618,#2618,#2312,.T.);
#3123=EDGE_CURVE('',#2618,#2617,#1649,.T.);
#3124=EDGE_CURVE('',#2619,#2619,#2313,.T.);
#3125=EDGE_CURVE('',#2620,#2620,#2314,.T.);
#3126=EDGE_CURVE('',#2620,#2619,#1650,.T.);
#3127=EDGE_CURVE('',#2621,#2621,#2315,.T.);
#3128=EDGE_CURVE('',#2621,#2611,#1651,.T.);
#3129=EDGE_CURVE('',#2622,#2623,#2316,.T.);
#3130=EDGE_CURVE('',#2624,#2622,#1652,.T.);
#3131=EDGE_CURVE('',#2625,#2624,#2317,.T.);
#3132=EDGE_CURVE('',#2623,#2625,#1653,.T.);
#3133=EDGE_CURVE('',#2623,#2626,#1654,.T.);
#3134=EDGE_CURVE('',#2627,#2625,#1655,.T.);
#3135=EDGE_CURVE('',#2627,#2626,#1656,.T.);
#3136=EDGE_CURVE('',#2626,#2628,#2318,.T.);
#3137=EDGE_CURVE('',#2629,#2627,#2319,.T.);
#3138=EDGE_CURVE('',#2628,#2629,#1657,.T.);
#3139=EDGE_CURVE('',#2628,#2622,#1658,.T.);
#3140=EDGE_CURVE('',#2624,#2629,#1659,.T.);
#3141=EDGE_CURVE('',#2630,#2630,#2320,.T.);
#3142=EDGE_CURVE('',#2631,#2631,#2321,.T.);
#3143=EDGE_CURVE('',#2632,#2632,#2322,.T.);
#3144=EDGE_CURVE('',#2632,#2630,#1660,.T.);
#3145=EDGE_CURVE('',#2633,#2633,#2323,.T.);
#3146=EDGE_CURVE('',#2633,#2631,#1661,.T.);
#3147=EDGE_CURVE('',#2634,#2634,#2324,.T.);
#3148=EDGE_CURVE('',#2635,#2635,#2325,.T.);
#3149=EDGE_CURVE('',#2635,#2634,#1662,.T.);
#3150=EDGE_CURVE('',#2636,#2636,#2326,.T.);
#3151=EDGE_CURVE('',#2636,#2635,#1663,.T.);
#3152=EDGE_CURVE('',#2637,#2637,#2327,.T.);
#3153=EDGE_CURVE('',#2637,#2636,#1664,.T.);
#3154=EDGE_CURVE('',#2638,#2638,#2328,.T.);
#3155=EDGE_CURVE('',#2639,#2639,#2329,.F.);
#3156=EDGE_CURVE('',#2639,#2638,#1665,.T.);
#3157=EDGE_CURVE('',#2640,#2640,#2330,.F.);
#3158=EDGE_CURVE('',#2640,#2639,#1666,.T.);
#3159=EDGE_CURVE('',#2641,#2641,#2331,.T.);
#3160=EDGE_CURVE('',#2641,#2640,#1667,.T.);
#3161=EDGE_CURVE('',#2642,#2643,#1668,.T.);
#3162=EDGE_CURVE('',#2643,#2644,#1669,.T.);
#3163=EDGE_CURVE('',#2644,#2645,#1670,.T.);
#3164=EDGE_CURVE('',#2642,#2645,#1671,.T.);
#3165=EDGE_CURVE('',#2643,#2646,#1672,.T.);
#3166=EDGE_CURVE('',#2646,#2647,#1673,.T.);
#3167=EDGE_CURVE('',#2647,#2644,#1674,.T.);
#3168=EDGE_CURVE('',#2646,#2648,#1675,.T.);
#3169=EDGE_CURVE('',#2648,#2649,#1676,.T.);
#3170=EDGE_CURVE('',#2649,#2647,#1677,.T.);
#3171=EDGE_CURVE('',#2648,#2650,#1678,.T.);
#3172=EDGE_CURVE('',#2650,#2651,#1679,.T.);
#3173=EDGE_CURVE('',#2651,#2649,#1680,.T.);
#3174=EDGE_CURVE('',#2650,#2652,#1681,.T.);
#3175=EDGE_CURVE('',#2652,#2653,#1682,.T.);
#3176=EDGE_CURVE('',#2653,#2651,#1683,.T.);
#3177=EDGE_CURVE('',#2652,#2642,#1684,.T.);
#3178=EDGE_CURVE('',#2645,#2653,#1685,.T.);
#3179=EDGE_CURVE('',#2654,#2654,#2332,.T.);
#3180=EDGE_CURVE('',#2654,#2655,#1686,.T.);
#3181=EDGE_CURVE('',#2655,#2655,#2333,.T.);
#3182=EDGE_CURVE('',#2656,#2656,#2334,.T.);
#3183=EDGE_CURVE('',#2657,#2658,#1687,.T.);
#3184=EDGE_CURVE('',#2658,#2659,#1688,.T.);
#3185=EDGE_CURVE('',#2659,#2660,#1689,.T.);
#3186=EDGE_CURVE('',#2660,#2661,#1690,.T.);
#3187=EDGE_CURVE('',#2661,#2662,#1691,.T.);
#3188=EDGE_CURVE('',#2662,#2657,#1692,.T.);
#3189=EDGE_CURVE('',#2663,#2663,#2335,.T.);
#3190=EDGE_CURVE('',#2664,#2665,#1693,.T.);
#3191=EDGE_CURVE('',#2666,#2664,#1694,.T.);
#3192=EDGE_CURVE('',#2667,#2666,#1695,.T.);
#3193=EDGE_CURVE('',#2668,#2667,#1696,.T.);
#3194=EDGE_CURVE('',#2669,#2668,#1697,.T.);
#3195=EDGE_CURVE('',#2665,#2669,#1698,.T.);
#3196=EDGE_CURVE('',#2670,#2670,#2336,.T.);
#3197=EDGE_CURVE('',#2664,#2657,#1699,.T.);
#3198=EDGE_CURVE('',#2666,#2662,#1700,.T.);
#3199=EDGE_CURVE('',#2667,#2661,#1701,.T.);
#3200=EDGE_CURVE('',#2668,#2660,#1702,.T.);
#3201=EDGE_CURVE('',#2669,#2659,#1703,.T.);
#3202=EDGE_CURVE('',#2665,#2658,#1704,.T.);
#3203=EDGE_CURVE('',#2671,#2671,#2337,.T.);
#3204=EDGE_CURVE('',#2671,#2672,#1705,.T.);
#3205=EDGE_CURVE('',#2672,#2672,#2338,.T.);
#3206=EDGE_CURVE('',#2673,#2673,#2339,.T.);
#3207=EDGE_CURVE('',#2663,#2673,#1706,.T.);
#3208=EDGE_CURVE('',#2674,#2674,#2340,.T.);
#3209=EDGE_CURVE('',#2674,#2670,#1707,.T.);
#3210=EDGE_CURVE('',#2675,#2675,#2341,.T.);
#3211=EDGE_CURVE('',#2675,#2656,#1708,.T.);
#3212=EDGE_CURVE('',#2676,#2676,#2342,.T.);
#3213=EDGE_CURVE('',#2677,#2677,#2343,.T.);
#3214=EDGE_CURVE('',#2678,#2678,#2344,.T.);
#3215=EDGE_CURVE('',#2678,#2676,#1709,.T.);
#3216=EDGE_CURVE('',#2679,#2679,#2345,.T.);
#3217=EDGE_CURVE('',#2680,#2680,#2346,.T.);
#3218=EDGE_CURVE('',#2680,#2679,#1710,.T.);
#3219=EDGE_CURVE('',#2681,#2681,#2347,.T.);
#3220=EDGE_CURVE('',#2681,#2677,#1711,.T.);
#3221=EDGE_CURVE('',#2682,#2682,#2348,.T.);
#3222=EDGE_CURVE('',#2682,#2683,#1712,.T.);
#3223=EDGE_CURVE('',#2683,#2683,#2349,.T.);
#3224=EDGE_CURVE('',#2683,#2684,#1713,.T.);
#3225=EDGE_CURVE('',#2684,#2684,#2350,.T.);
#3226=EDGE_CURVE('',#2685,#2685,#2351,.T.);
#3227=EDGE_CURVE('',#2685,#2686,#1714,.T.);
#3228=EDGE_CURVE('',#2686,#2686,#2352,.T.);
#3229=EDGE_CURVE('',#2687,#2688,#11,.T.);
#3230=EDGE_CURVE('',#2689,#2687,#12,.T.);
#3231=EDGE_CURVE('',#2689,#2690,#1715,.T.);
#3232=EDGE_CURVE('',#2690,#2690,#2353,.T.);
#3233=EDGE_CURVE('',#2691,#2689,#13,.T.);
#3234=EDGE_CURVE('',#2692,#2691,#14,.T.);
#3235=EDGE_CURVE('',#2693,#2692,#15,.T.);
#3236=EDGE_CURVE('',#2688,#2693,#16,.T.);
#3237=EDGE_CURVE('',#2694,#2694,#2354,.T.);
#3238=EDGE_CURVE('',#2694,#2695,#1716,.T.);
#3239=EDGE_CURVE('',#2696,#2695,#17,.T.);
#3240=EDGE_CURVE('',#2697,#2696,#18,.T.);
#3241=EDGE_CURVE('',#2698,#2697,#19,.T.);
#3242=EDGE_CURVE('',#2699,#2698,#20,.T.);
#3243=EDGE_CURVE('',#2700,#2699,#21,.T.);
#3244=EDGE_CURVE('',#2695,#2700,#22,.T.);
#3245=EDGE_CURVE('',#2691,#2700,#1717,.T.);
#3246=EDGE_CURVE('',#2692,#2699,#1718,.T.);
#3247=EDGE_CURVE('',#2689,#2695,#1719,.T.);
#3248=EDGE_CURVE('',#2687,#2696,#1720,.T.);
#3249=EDGE_CURVE('',#2701,#2701,#2355,.F.);
#3250=EDGE_CURVE('',#2701,#2702,#1721,.T.);
#3251=EDGE_CURVE('',#2702,#2702,#2356,.F.);
#3252=EDGE_CURVE('',#2688,#2697,#1722,.T.);
#3253=EDGE_CURVE('',#2693,#2698,#1723,.T.);
#3254=EDGE_CURVE('',#2703,#2703,#2357,.T.);
#3255=EDGE_CURVE('',#2703,#2704,#1724,.T.);
#3256=EDGE_CURVE('',#2704,#2704,#2358,.T.);
#3257=EDGE_CURVE('',#2705,#2705,#2359,.T.);
#3258=EDGE_CURVE('',#2706,#2706,#2360,.T.);
#3259=EDGE_CURVE('',#2706,#2705,#1725,.T.);
#3260=EDGE_CURVE('',#2707,#2708,#1726,.T.);
#3261=EDGE_CURVE('',#2709,#2707,#1727,.T.);
#3262=EDGE_CURVE('',#2710,#2709,#1728,.T.);
#3263=EDGE_CURVE('',#2710,#2708,#1729,.T.);
#3264=EDGE_CURVE('',#2711,#2710,#1730,.T.);
#3265=EDGE_CURVE('',#2712,#2709,#1731,.T.);
#3266=EDGE_CURVE('',#2711,#2712,#1732,.T.);
#3267=EDGE_CURVE('',#2713,#2711,#1733,.T.);
#3268=EDGE_CURVE('',#2714,#2712,#1734,.T.);
#3269=EDGE_CURVE('',#2713,#2714,#1735,.T.);
#3270=EDGE_CURVE('',#2715,#2716,#1736,.T.);
#3271=EDGE_CURVE('',#2715,#2713,#1737,.T.);
#3272=EDGE_CURVE('',#2716,#2714,#1738,.T.);
#3273=EDGE_CURVE('',#2716,#2717,#1739,.T.);
#3274=EDGE_CURVE('',#2717,#2707,#1740,.T.);
#3275=EDGE_CURVE('',#2717,#2718,#1741,.T.);
#3276=EDGE_CURVE('',#2719,#2718,#1742,.T.);
#3277=EDGE_CURVE('',#2720,#2719,#1743,.T.);
#3278=EDGE_CURVE('',#2720,#2715,#1744,.T.);
#3279=EDGE_CURVE('',#2708,#2721,#1745,.T.);
#3280=EDGE_CURVE('',#2721,#2722,#1746,.T.);
#3281=EDGE_CURVE('',#2722,#2723,#1747,.T.);
#3282=EDGE_CURVE('',#2723,#2724,#1748,.T.);
#3283=EDGE_CURVE('',#2724,#2725,#1749,.T.);
#3284=EDGE_CURVE('',#2725,#2726,#1750,.T.);
#3285=EDGE_CURVE('',#2726,#2727,#1751,.T.);
#3286=EDGE_CURVE('',#2727,#2728,#1752,.T.);
#3287=EDGE_CURVE('',#2718,#2728,#1753,.T.);
#3288=EDGE_CURVE('',#2729,#2730,#1754,.T.);
#3289=EDGE_CURVE('',#2729,#2730,#2361,.T.);
#3290=EDGE_CURVE('',#2731,#2729,#287,.T.);
#3291=EDGE_CURVE('',#2732,#2731,#2362,.T.);
#3292=EDGE_CURVE('',#2733,#2732,#288,.T.);
#3293=EDGE_CURVE('',#2733,#2734,#1755,.T.);
#3294=EDGE_CURVE('',#2735,#2734,#289,.T.);
#3295=EDGE_CURVE('',#2734,#2735,#290,.T.);
#3296=EDGE_CURVE('',#2730,#2733,#291,.T.);
#3297=EDGE_CURVE('',#2732,#2731,#1756,.T.);
#3298=EDGE_CURVE('',#2736,#2723,#2363,.T.);
#3299=EDGE_CURVE('',#2737,#2736,#1757,.T.);
#3300=EDGE_CURVE('',#2738,#2737,#2364,.T.);
#3301=EDGE_CURVE('',#2724,#2738,#2365,.T.);
#3302=EDGE_CURVE('',#2739,#2739,#2366,.T.);
#3303=EDGE_CURVE('',#2739,#2738,#1758,.T.);
#3304=EDGE_CURVE('',#2740,#2737,#1759,.T.);
#3305=EDGE_CURVE('',#2741,#2740,#2367,.T.);
#3306=EDGE_CURVE('',#2736,#2741,#1760,.T.);
#3307=EDGE_CURVE('',#2725,#2722,#2368,.T.);
#3308=EDGE_CURVE('',#2741,#2742,#1761,.T.);
#3309=EDGE_CURVE('',#2742,#2720,#1762,.T.);
#3310=EDGE_CURVE('',#2743,#2719,#1763,.T.);
#3311=EDGE_CURVE('',#2744,#2743,#1764,.T.);
#3312=EDGE_CURVE('',#2744,#2745,#1765,.T.);
#3313=EDGE_CURVE('',#2745,#2740,#1766,.T.);
#3314=EDGE_CURVE('',#2721,#2726,#2369,.T.);
#3315=EDGE_CURVE('',#2745,#2742,#2370,.T.);
#3316=EDGE_CURVE('',#2726,#2746,#2371,.T.);
#3317=EDGE_CURVE('',#2742,#2721,#2372,.T.);
#3318=EDGE_CURVE('',#2746,#2745,#2373,.T.);
#3319=EDGE_CURVE('',#2746,#2747,#1767,.T.);
#3320=EDGE_CURVE('',#2747,#2747,#2374,.T.);
#3321=EDGE_CURVE('',#2727,#2744,#1768,.T.);
#3322=EDGE_CURVE('',#2728,#2743,#1769,.T.);
#3323=EDGE_CURVE('',#2748,#2748,#2375,.T.);
#3324=EDGE_CURVE('',#2748,#2749,#1770,.T.);
#3325=EDGE_CURVE('',#2749,#2749,#2376,.T.);
#3326=EDGE_CURVE('',#2750,#2750,#2377,.T.);
#3327=EDGE_CURVE('',#2750,#2751,#1771,.T.);
#3328=EDGE_CURVE('',#2751,#2751,#2378,.T.);
#3329=EDGE_CURVE('',#2752,#2752,#2379,.T.);
#3330=EDGE_CURVE('',#2752,#2753,#1772,.T.);
#3331=EDGE_CURVE('',#2753,#2753,#2380,.T.);
#3332=EDGE_CURVE('',#2754,#2754,#2381,.T.);
#3333=EDGE_CURVE('',#2754,#2755,#1773,.T.);
#3334=EDGE_CURVE('',#2755,#2755,#2382,.T.);
#3335=EDGE_CURVE('',#2756,#2756,#2383,.T.);
#3336=EDGE_CURVE('',#2757,#2757,#2384,.T.);
#3337=EDGE_CURVE('',#2757,#2758,#1774,.T.);
#3338=EDGE_CURVE('',#2758,#2758,#2385,.T.);
#3339=EDGE_CURVE('',#2759,#2759,#2386,.T.);
#3340=EDGE_CURVE('',#2759,#2760,#1775,.T.);
#3341=EDGE_CURVE('',#2760,#2760,#2387,.T.);
#3342=EDGE_CURVE('',#2761,#2761,#2388,.T.);
#3343=EDGE_CURVE('',#2761,#2756,#1776,.T.);
#3344=EDGE_CURVE('',#2762,#2762,#2389,.T.);
#3345=EDGE_CURVE('',#2762,#2763,#1777,.T.);
#3346=EDGE_CURVE('',#2763,#2763,#2390,.T.);
#3347=EDGE_CURVE('',#2764,#2764,#2391,.T.);
#3348=EDGE_CURVE('',#2764,#2765,#1778,.T.);
#3349=EDGE_CURVE('',#2765,#2765,#2392,.T.);
#3350=EDGE_CURVE('',#2766,#2766,#2393,.T.);
#3351=EDGE_CURVE('',#2767,#2767,#2394,.T.);
#3352=EDGE_CURVE('',#2767,#2768,#1779,.T.);
#3353=EDGE_CURVE('',#2768,#2768,#2395,.T.);
#3354=EDGE_CURVE('',#2766,#2767,#1780,.T.);
#3355=EDGE_CURVE('',#2769,#2769,#2396,.T.);
#3356=EDGE_CURVE('',#2770,#2771,#1781,.T.);
#3357=EDGE_CURVE('',#2770,#2772,#1782,.T.);
#3358=EDGE_CURVE('',#2772,#2773,#1783,.T.);
#3359=EDGE_CURVE('',#2771,#2773,#1784,.T.);
#3360=EDGE_CURVE('',#2774,#2770,#1785,.T.);
#3361=EDGE_CURVE('',#2774,#2775,#1786,.T.);
#3362=EDGE_CURVE('',#2775,#2772,#1787,.T.);
#3363=EDGE_CURVE('',#2776,#2774,#1788,.T.);
#3364=EDGE_CURVE('',#2776,#2777,#1789,.T.);
#3365=EDGE_CURVE('',#2777,#2775,#1790,.T.);
#3366=EDGE_CURVE('',#2778,#2776,#1791,.T.);
#3367=EDGE_CURVE('',#2778,#2779,#1792,.T.);
#3368=EDGE_CURVE('',#2779,#2777,#1793,.T.);
#3369=EDGE_CURVE('',#2780,#2778,#1794,.T.);
#3370=EDGE_CURVE('',#2780,#2781,#1795,.T.);
#3371=EDGE_CURVE('',#2781,#2779,#1796,.T.);
#3372=EDGE_CURVE('',#2771,#2780,#1797,.T.);
#3373=EDGE_CURVE('',#2773,#2781,#1798,.T.);
#3374=EDGE_CURVE('',#2782,#2782,#2397,.T.);
#3375=EDGE_CURVE('',#2783,#2783,#2398,.T.);
#3376=EDGE_CURVE('',#2783,#2782,#1799,.T.);
#3377=EDGE_CURVE('',#2769,#2783,#1800,.T.);
#3378=EDGE_CURVE('',#2784,#2784,#2399,.T.);
#3379=EDGE_CURVE('',#2785,#2785,#2400,.T.);
#3380=EDGE_CURVE('',#2785,#2784,#1801,.T.);
#3381=EDGE_CURVE('',#2786,#2786,#2401,.T.);
#3382=EDGE_CURVE('',#2786,#2785,#1802,.T.);
#3383=EDGE_CURVE('',#2787,#2787,#2402,.T.);
#3384=EDGE_CURVE('',#2787,#2786,#1803,.T.);
#3385=EDGE_CURVE('',#2788,#2788,#2403,.T.);
#3386=EDGE_CURVE('',#2789,#2789,#2404,.F.);
#3387=EDGE_CURVE('',#2789,#2788,#1804,.T.);
#3388=EDGE_CURVE('',#2790,#2790,#2405,.F.);
#3389=EDGE_CURVE('',#2790,#2789,#1805,.T.);
#3390=EDGE_CURVE('',#2791,#2791,#2406,.T.);
#3391=EDGE_CURVE('',#2791,#2790,#1806,.T.);
#3392=EDGE_CURVE('',#2792,#2793,#1807,.T.);
#3393=EDGE_CURVE('',#2793,#2794,#1808,.T.);
#3394=EDGE_CURVE('',#2794,#2795,#1809,.T.);
#3395=EDGE_CURVE('',#2792,#2795,#1810,.T.);
#3396=EDGE_CURVE('',#2793,#2796,#1811,.T.);
#3397=EDGE_CURVE('',#2796,#2797,#1812,.T.);
#3398=EDGE_CURVE('',#2797,#2794,#1813,.T.);
#3399=EDGE_CURVE('',#2796,#2798,#1814,.T.);
#3400=EDGE_CURVE('',#2798,#2799,#1815,.T.);
#3401=EDGE_CURVE('',#2799,#2797,#1816,.T.);
#3402=EDGE_CURVE('',#2798,#2800,#1817,.T.);
#3403=EDGE_CURVE('',#2800,#2801,#1818,.T.);
#3404=EDGE_CURVE('',#2801,#2799,#1819,.T.);
#3405=EDGE_CURVE('',#2800,#2802,#1820,.T.);
#3406=EDGE_CURVE('',#2802,#2803,#1821,.T.);
#3407=EDGE_CURVE('',#2803,#2801,#1822,.T.);
#3408=EDGE_CURVE('',#2802,#2792,#1823,.T.);
#3409=EDGE_CURVE('',#2795,#2803,#1824,.T.);
#3410=ORIENTED_EDGE('',*,*,#2804,.F.);
#3411=ORIENTED_EDGE('',*,*,#2805,.T.);
#3412=ORIENTED_EDGE('',*,*,#2806,.F.);
#3413=ORIENTED_EDGE('',*,*,#2805,.F.);
#3414=ORIENTED_EDGE('',*,*,#2807,.F.);
#3415=ORIENTED_EDGE('',*,*,#2808,.T.);
#3416=ORIENTED_EDGE('',*,*,#2809,.F.);
#3417=ORIENTED_EDGE('',*,*,#2808,.F.);
#3418=ORIENTED_EDGE('',*,*,#2810,.F.);
#3419=ORIENTED_EDGE('',*,*,#2811,.T.);
#3420=ORIENTED_EDGE('',*,*,#2812,.F.);
#3421=ORIENTED_EDGE('',*,*,#2811,.F.);
#3422=ORIENTED_EDGE('',*,*,#2813,.F.);
#3423=ORIENTED_EDGE('',*,*,#2814,.T.);
#3424=ORIENTED_EDGE('',*,*,#2815,.F.);
#3425=ORIENTED_EDGE('',*,*,#2814,.F.);
#3426=ORIENTED_EDGE('',*,*,#2816,.F.);
#3427=ORIENTED_EDGE('',*,*,#2817,.T.);
#3428=ORIENTED_EDGE('',*,*,#2818,.F.);
#3429=ORIENTED_EDGE('',*,*,#2817,.F.);
#3430=ORIENTED_EDGE('',*,*,#2819,.F.);
#3431=ORIENTED_EDGE('',*,*,#2820,.T.);
#3432=ORIENTED_EDGE('',*,*,#2821,.F.);
#3433=ORIENTED_EDGE('',*,*,#2820,.F.);
#3434=ORIENTED_EDGE('',*,*,#2822,.F.);
#3435=ORIENTED_EDGE('',*,*,#2823,.T.);
#3436=ORIENTED_EDGE('',*,*,#2824,.F.);
#3437=ORIENTED_EDGE('',*,*,#2823,.F.);
#3438=ORIENTED_EDGE('',*,*,#2825,.F.);
#3439=ORIENTED_EDGE('',*,*,#2826,.T.);
#3440=ORIENTED_EDGE('',*,*,#2827,.F.);
#3441=ORIENTED_EDGE('',*,*,#2826,.F.);
#3442=ORIENTED_EDGE('',*,*,#2828,.F.);
#3443=ORIENTED_EDGE('',*,*,#2829,.T.);
#3444=ORIENTED_EDGE('',*,*,#2830,.F.);
#3445=ORIENTED_EDGE('',*,*,#2829,.F.);
#3446=ORIENTED_EDGE('',*,*,#2831,.T.);
#3447=ORIENTED_EDGE('',*,*,#2832,.T.);
#3448=ORIENTED_EDGE('',*,*,#2833,.F.);
#3449=ORIENTED_EDGE('',*,*,#2834,.F.);
#3450=ORIENTED_EDGE('',*,*,#2835,.T.);
#3451=ORIENTED_EDGE('',*,*,#2834,.T.);
#3452=ORIENTED_EDGE('',*,*,#2836,.F.);
#3453=ORIENTED_EDGE('',*,*,#2837,.F.);
#3454=ORIENTED_EDGE('',*,*,#2838,.T.);
#3455=ORIENTED_EDGE('',*,*,#2837,.T.);
#3456=ORIENTED_EDGE('',*,*,#2839,.F.);
#3457=ORIENTED_EDGE('',*,*,#2840,.F.);
#3458=ORIENTED_EDGE('',*,*,#2841,.T.);
#3459=ORIENTED_EDGE('',*,*,#2840,.T.);
#3460=ORIENTED_EDGE('',*,*,#2842,.F.);
#3461=ORIENTED_EDGE('',*,*,#2832,.F.);
#3462=ORIENTED_EDGE('',*,*,#2842,.T.);
#3463=ORIENTED_EDGE('',*,*,#2839,.T.);
#3464=ORIENTED_EDGE('',*,*,#2836,.T.);
#3465=ORIENTED_EDGE('',*,*,#2833,.T.);
#3466=ORIENTED_EDGE('',*,*,#2830,.T.);
#3467=ORIENTED_EDGE('',*,*,#2827,.T.);
#3468=ORIENTED_EDGE('',*,*,#2824,.T.);
#3469=ORIENTED_EDGE('',*,*,#2821,.T.);
#3470=ORIENTED_EDGE('',*,*,#2818,.T.);
#3471=ORIENTED_EDGE('',*,*,#2815,.T.);
#3472=ORIENTED_EDGE('',*,*,#2812,.T.);
#3473=ORIENTED_EDGE('',*,*,#2809,.T.);
#3474=ORIENTED_EDGE('',*,*,#2806,.T.);
#3475=ORIENTED_EDGE('',*,*,#2841,.F.);
#3476=ORIENTED_EDGE('',*,*,#2831,.F.);
#3477=ORIENTED_EDGE('',*,*,#2835,.F.);
#3478=ORIENTED_EDGE('',*,*,#2838,.F.);
#3479=ORIENTED_EDGE('',*,*,#2828,.T.);
#3480=ORIENTED_EDGE('',*,*,#2825,.T.);
#3481=ORIENTED_EDGE('',*,*,#2822,.T.);
#3482=ORIENTED_EDGE('',*,*,#2819,.T.);
#3483=ORIENTED_EDGE('',*,*,#2816,.T.);
#3484=ORIENTED_EDGE('',*,*,#2813,.T.);
#3485=ORIENTED_EDGE('',*,*,#2810,.T.);
#3486=ORIENTED_EDGE('',*,*,#2807,.T.);
#3487=ORIENTED_EDGE('',*,*,#2804,.T.);
#3488=ORIENTED_EDGE('',*,*,#2843,.T.);
#3489=ORIENTED_EDGE('',*,*,#2844,.T.);
#3490=ORIENTED_EDGE('',*,*,#2845,.F.);
#3491=ORIENTED_EDGE('',*,*,#2846,.F.);
#3492=ORIENTED_EDGE('',*,*,#2847,.T.);
#3493=ORIENTED_EDGE('',*,*,#2846,.T.);
#3494=ORIENTED_EDGE('',*,*,#2848,.F.);
#3495=ORIENTED_EDGE('',*,*,#2849,.F.);
#3496=ORIENTED_EDGE('',*,*,#2850,.T.);
#3497=ORIENTED_EDGE('',*,*,#2849,.T.);
#3498=ORIENTED_EDGE('',*,*,#2851,.F.);
#3499=ORIENTED_EDGE('',*,*,#2852,.F.);
#3500=ORIENTED_EDGE('',*,*,#2853,.T.);
#3501=ORIENTED_EDGE('',*,*,#2852,.T.);
#3502=ORIENTED_EDGE('',*,*,#2854,.F.);
#3503=ORIENTED_EDGE('',*,*,#2844,.F.);
#3504=ORIENTED_EDGE('',*,*,#2854,.T.);
#3505=ORIENTED_EDGE('',*,*,#2851,.T.);
#3506=ORIENTED_EDGE('',*,*,#2848,.T.);
#3507=ORIENTED_EDGE('',*,*,#2845,.T.);
#3508=ORIENTED_EDGE('',*,*,#2853,.F.);
#3509=ORIENTED_EDGE('',*,*,#2843,.F.);
#3510=ORIENTED_EDGE('',*,*,#2847,.F.);
#3511=ORIENTED_EDGE('',*,*,#2850,.F.);
#3512=ORIENTED_EDGE('',*,*,#2855,.T.);
#3513=ORIENTED_EDGE('',*,*,#2856,.T.);
#3514=ORIENTED_EDGE('',*,*,#2857,.F.);
#3515=ORIENTED_EDGE('',*,*,#2858,.F.);
#3516=ORIENTED_EDGE('',*,*,#2859,.T.);
#3517=ORIENTED_EDGE('',*,*,#2858,.T.);
#3518=ORIENTED_EDGE('',*,*,#2860,.F.);
#3519=ORIENTED_EDGE('',*,*,#2861,.F.);
#3520=ORIENTED_EDGE('',*,*,#2862,.T.);
#3521=ORIENTED_EDGE('',*,*,#2861,.T.);
#3522=ORIENTED_EDGE('',*,*,#2863,.F.);
#3523=ORIENTED_EDGE('',*,*,#2864,.F.);
#3524=ORIENTED_EDGE('',*,*,#2865,.T.);
#3525=ORIENTED_EDGE('',*,*,#2864,.T.);
#3526=ORIENTED_EDGE('',*,*,#2866,.F.);
#3527=ORIENTED_EDGE('',*,*,#2856,.F.);
#3528=ORIENTED_EDGE('',*,*,#2866,.T.);
#3529=ORIENTED_EDGE('',*,*,#2863,.T.);
#3530=ORIENTED_EDGE('',*,*,#2860,.T.);
#3531=ORIENTED_EDGE('',*,*,#2857,.T.);
#3532=ORIENTED_EDGE('',*,*,#2865,.F.);
#3533=ORIENTED_EDGE('',*,*,#2855,.F.);
#3534=ORIENTED_EDGE('',*,*,#2859,.F.);
#3535=ORIENTED_EDGE('',*,*,#2862,.F.);
#3536=ORIENTED_EDGE('',*,*,#2867,.F.);
#3537=ORIENTED_EDGE('',*,*,#2868,.T.);
#3538=ORIENTED_EDGE('',*,*,#2869,.F.);
#3539=ORIENTED_EDGE('',*,*,#2868,.F.);
#3540=ORIENTED_EDGE('',*,*,#2867,.T.);
#3541=ORIENTED_EDGE('',*,*,#2870,.F.);
#3542=ORIENTED_EDGE('',*,*,#2871,.T.);
#3543=ORIENTED_EDGE('',*,*,#2872,.F.);
#3544=ORIENTED_EDGE('',*,*,#2871,.F.);
#3545=ORIENTED_EDGE('',*,*,#2870,.T.);
#3546=ORIENTED_EDGE('',*,*,#2873,.F.);
#3547=ORIENTED_EDGE('',*,*,#2874,.T.);
#3548=ORIENTED_EDGE('',*,*,#2875,.F.);
#3549=ORIENTED_EDGE('',*,*,#2874,.F.);
#3550=ORIENTED_EDGE('',*,*,#2873,.T.);
#3551=ORIENTED_EDGE('',*,*,#2876,.F.);
#3552=ORIENTED_EDGE('',*,*,#2877,.T.);
#3553=ORIENTED_EDGE('',*,*,#2878,.F.);
#3554=ORIENTED_EDGE('',*,*,#2877,.F.);
#3555=ORIENTED_EDGE('',*,*,#2876,.T.);
#3556=ORIENTED_EDGE('',*,*,#2879,.F.);
#3557=ORIENTED_EDGE('',*,*,#2880,.T.);
#3558=ORIENTED_EDGE('',*,*,#2881,.T.);
#3559=ORIENTED_EDGE('',*,*,#2880,.F.);
#3560=ORIENTED_EDGE('',*,*,#2881,.F.);
#3561=ORIENTED_EDGE('',*,*,#2882,.F.);
#3562=ORIENTED_EDGE('',*,*,#2883,.T.);
#3563=ORIENTED_EDGE('',*,*,#2884,.T.);
#3564=ORIENTED_EDGE('',*,*,#2883,.F.);
#3565=ORIENTED_EDGE('',*,*,#2884,.F.);
#3566=ORIENTED_EDGE('',*,*,#2885,.F.);
#3567=ORIENTED_EDGE('',*,*,#2886,.T.);
#3568=ORIENTED_EDGE('',*,*,#2887,.T.);
#3569=ORIENTED_EDGE('',*,*,#2886,.F.);
#3570=ORIENTED_EDGE('',*,*,#2887,.F.);
#3571=ORIENTED_EDGE('',*,*,#2888,.F.);
#3572=ORIENTED_EDGE('',*,*,#2889,.T.);
#3573=ORIENTED_EDGE('',*,*,#2890,.T.);
#3574=ORIENTED_EDGE('',*,*,#2889,.F.);
#3575=ORIENTED_EDGE('',*,*,#2890,.F.);
#3576=ORIENTED_EDGE('',*,*,#2891,.F.);
#3577=ORIENTED_EDGE('',*,*,#2892,.T.);
#3578=ORIENTED_EDGE('',*,*,#2893,.F.);
#3579=ORIENTED_EDGE('',*,*,#2892,.F.);
#3580=ORIENTED_EDGE('',*,*,#2891,.T.);
#3581=ORIENTED_EDGE('',*,*,#2894,.F.);
#3582=ORIENTED_EDGE('',*,*,#2895,.F.);
#3583=ORIENTED_EDGE('',*,*,#2896,.T.);
#3584=ORIENTED_EDGE('',*,*,#2894,.T.);
#3585=ORIENTED_EDGE('',*,*,#2896,.F.);
#3586=ORIENTED_EDGE('',*,*,#2897,.T.);
#3587=ORIENTED_EDGE('',*,*,#2898,.T.);
#3588=ORIENTED_EDGE('',*,*,#2899,.F.);
#3589=ORIENTED_EDGE('',*,*,#2900,.F.);
#3590=ORIENTED_EDGE('',*,*,#2901,.T.);
#3591=ORIENTED_EDGE('',*,*,#2900,.T.);
#3592=ORIENTED_EDGE('',*,*,#2902,.F.);
#3593=ORIENTED_EDGE('',*,*,#2903,.F.);
#3594=ORIENTED_EDGE('',*,*,#2904,.T.);
#3595=ORIENTED_EDGE('',*,*,#2903,.T.);
#3596=ORIENTED_EDGE('',*,*,#2905,.F.);
#3597=ORIENTED_EDGE('',*,*,#2906,.F.);
#3598=ORIENTED_EDGE('',*,*,#2907,.T.);
#3599=ORIENTED_EDGE('',*,*,#2906,.T.);
#3600=ORIENTED_EDGE('',*,*,#2908,.F.);
#3601=ORIENTED_EDGE('',*,*,#2898,.F.);
#3602=ORIENTED_EDGE('',*,*,#2908,.T.);
#3603=ORIENTED_EDGE('',*,*,#2905,.T.);
#3604=ORIENTED_EDGE('',*,*,#2902,.T.);
#3605=ORIENTED_EDGE('',*,*,#2899,.T.);
#3606=ORIENTED_EDGE('',*,*,#2893,.T.);
#3607=ORIENTED_EDGE('',*,*,#2878,.T.);
#3608=ORIENTED_EDGE('',*,*,#2875,.T.);
#3609=ORIENTED_EDGE('',*,*,#2872,.T.);
#3610=ORIENTED_EDGE('',*,*,#2869,.T.);
#3611=ORIENTED_EDGE('',*,*,#2907,.F.);
#3612=ORIENTED_EDGE('',*,*,#2897,.F.);
#3613=ORIENTED_EDGE('',*,*,#2901,.F.);
#3614=ORIENTED_EDGE('',*,*,#2904,.F.);
#3615=ORIENTED_EDGE('',*,*,#2895,.T.);
#3616=ORIENTED_EDGE('',*,*,#2888,.T.);
#3617=ORIENTED_EDGE('',*,*,#2885,.T.);
#3618=ORIENTED_EDGE('',*,*,#2882,.T.);
#3619=ORIENTED_EDGE('',*,*,#2879,.T.);
#3620=ORIENTED_EDGE('',*,*,#2909,.F.);
#3621=ORIENTED_EDGE('',*,*,#2910,.T.);
#3622=ORIENTED_EDGE('',*,*,#2911,.F.);
#3623=ORIENTED_EDGE('',*,*,#2910,.F.);
#3624=ORIENTED_EDGE('',*,*,#2909,.T.);
#3625=ORIENTED_EDGE('',*,*,#2912,.F.);
#3626=ORIENTED_EDGE('',*,*,#2913,.F.);
#3627=ORIENTED_EDGE('',*,*,#2914,.T.);
#3628=ORIENTED_EDGE('',*,*,#2915,.F.);
#3629=ORIENTED_EDGE('',*,*,#2914,.F.);
#3630=ORIENTED_EDGE('',*,*,#2913,.T.);
#3631=ORIENTED_EDGE('',*,*,#2916,.F.);
#3632=ORIENTED_EDGE('',*,*,#2917,.F.);
#3633=ORIENTED_EDGE('',*,*,#2918,.T.);
#3634=ORIENTED_EDGE('',*,*,#2919,.F.);
#3635=ORIENTED_EDGE('',*,*,#2918,.F.);
#3636=ORIENTED_EDGE('',*,*,#2917,.T.);
#3637=ORIENTED_EDGE('',*,*,#2920,.F.);
#3638=ORIENTED_EDGE('',*,*,#2921,.F.);
#3639=ORIENTED_EDGE('',*,*,#2922,.T.);
#3640=ORIENTED_EDGE('',*,*,#2923,.F.);
#3641=ORIENTED_EDGE('',*,*,#2922,.F.);
#3642=ORIENTED_EDGE('',*,*,#2921,.T.);
#3643=ORIENTED_EDGE('',*,*,#2924,.F.);
#3644=ORIENTED_EDGE('',*,*,#2925,.F.);
#3645=ORIENTED_EDGE('',*,*,#2926,.T.);
#3646=ORIENTED_EDGE('',*,*,#2912,.T.);
#3647=ORIENTED_EDGE('',*,*,#2926,.F.);
#3648=ORIENTED_EDGE('',*,*,#2927,.F.);
#3649=ORIENTED_EDGE('',*,*,#2928,.T.);
#3650=ORIENTED_EDGE('',*,*,#2916,.T.);
#3651=ORIENTED_EDGE('',*,*,#2928,.F.);
#3652=ORIENTED_EDGE('',*,*,#2929,.F.);
#3653=ORIENTED_EDGE('',*,*,#2930,.T.);
#3654=ORIENTED_EDGE('',*,*,#2920,.T.);
#3655=ORIENTED_EDGE('',*,*,#2930,.F.);
#3656=ORIENTED_EDGE('',*,*,#2931,.F.);
#3657=ORIENTED_EDGE('',*,*,#2932,.T.);
#3658=ORIENTED_EDGE('',*,*,#2924,.T.);
#3659=ORIENTED_EDGE('',*,*,#2932,.F.);
#3660=ORIENTED_EDGE('',*,*,#2933,.F.);
#3661=ORIENTED_EDGE('',*,*,#2934,.T.);
#3662=ORIENTED_EDGE('',*,*,#2935,.T.);
#3663=ORIENTED_EDGE('',*,*,#2934,.F.);
#3664=ORIENTED_EDGE('',*,*,#2935,.F.);
#3665=ORIENTED_EDGE('',*,*,#2936,.F.);
#3666=ORIENTED_EDGE('',*,*,#2937,.F.);
#3667=ORIENTED_EDGE('',*,*,#2938,.T.);
#3668=ORIENTED_EDGE('',*,*,#2936,.T.);
#3669=ORIENTED_EDGE('',*,*,#2938,.F.);
#3670=ORIENTED_EDGE('',*,*,#2939,.F.);
#3671=ORIENTED_EDGE('',*,*,#2940,.T.);
#3672=ORIENTED_EDGE('',*,*,#2941,.T.);
#3673=ORIENTED_EDGE('',*,*,#2940,.F.);
#3674=ORIENTED_EDGE('',*,*,#2939,.T.);
#3675=ORIENTED_EDGE('',*,*,#2937,.T.);
#3676=ORIENTED_EDGE('',*,*,#2923,.T.);
#3677=ORIENTED_EDGE('',*,*,#2919,.T.);
#3678=ORIENTED_EDGE('',*,*,#2915,.T.);
#3679=ORIENTED_EDGE('',*,*,#2911,.T.);
#3680=ORIENTED_EDGE('',*,*,#2941,.F.);
#3681=ORIENTED_EDGE('',*,*,#2933,.T.);
#3682=ORIENTED_EDGE('',*,*,#2931,.T.);
#3683=ORIENTED_EDGE('',*,*,#2929,.T.);
#3684=ORIENTED_EDGE('',*,*,#2927,.T.);
#3685=ORIENTED_EDGE('',*,*,#2925,.T.);
#3686=ORIENTED_EDGE('',*,*,#2942,.F.);
#3687=ORIENTED_EDGE('',*,*,#2943,.T.);
#3688=ORIENTED_EDGE('',*,*,#2944,.T.);
#3689=ORIENTED_EDGE('',*,*,#2943,.F.);
#3690=ORIENTED_EDGE('',*,*,#2945,.F.);
#3691=ORIENTED_EDGE('',*,*,#2946,.T.);
#3692=ORIENTED_EDGE('',*,*,#2947,.T.);
#3693=ORIENTED_EDGE('',*,*,#2946,.F.);
#3694=ORIENTED_EDGE('',*,*,#2945,.T.);
#3695=ORIENTED_EDGE('',*,*,#2942,.T.);
#3696=ORIENTED_EDGE('',*,*,#2947,.F.);
#3697=ORIENTED_EDGE('',*,*,#2944,.F.);
#3698=ORIENTED_EDGE('',*,*,#2948,.T.);
#3699=ORIENTED_EDGE('',*,*,#2949,.T.);
#3700=ORIENTED_EDGE('',*,*,#2950,.F.);
#3701=ORIENTED_EDGE('',*,*,#2949,.F.);
#3702=ORIENTED_EDGE('',*,*,#2950,.T.);
#3703=ORIENTED_EDGE('',*,*,#2948,.F.);
#3704=ORIENTED_EDGE('',*,*,#2951,.F.);
#3705=ORIENTED_EDGE('',*,*,#2952,.T.);
#3706=ORIENTED_EDGE('',*,*,#2953,.T.);
#3707=ORIENTED_EDGE('',*,*,#2952,.F.);
#3708=ORIENTED_EDGE('',*,*,#2953,.F.);
#3709=ORIENTED_EDGE('',*,*,#2954,.F.);
#3710=ORIENTED_EDGE('',*,*,#2955,.F.);
#3711=ORIENTED_EDGE('',*,*,#2956,.F.);
#3712=ORIENTED_EDGE('',*,*,#2957,.F.);
#3713=ORIENTED_EDGE('',*,*,#2958,.F.);
#3714=ORIENTED_EDGE('',*,*,#2959,.F.);
#3715=ORIENTED_EDGE('',*,*,#2957,.T.);
#3716=ORIENTED_EDGE('',*,*,#2960,.T.);
#3717=ORIENTED_EDGE('',*,*,#2961,.F.);
#3718=ORIENTED_EDGE('',*,*,#2962,.F.);
#3719=ORIENTED_EDGE('',*,*,#2958,.T.);
#3720=ORIENTED_EDGE('',*,*,#2962,.T.);
#3721=ORIENTED_EDGE('',*,*,#2963,.F.);
#3722=ORIENTED_EDGE('',*,*,#2964,.F.);
#3723=ORIENTED_EDGE('',*,*,#2965,.F.);
#3724=ORIENTED_EDGE('',*,*,#2966,.T.);
#3725=ORIENTED_EDGE('',*,*,#2967,.T.);
#3726=ORIENTED_EDGE('',*,*,#2959,.T.);
#3727=ORIENTED_EDGE('',*,*,#2964,.T.);
#3728=ORIENTED_EDGE('',*,*,#2968,.F.);
#3729=ORIENTED_EDGE('',*,*,#2969,.F.);
#3730=ORIENTED_EDGE('',*,*,#2970,.T.);
#3731=ORIENTED_EDGE('',*,*,#2965,.T.);
#3732=ORIENTED_EDGE('',*,*,#2971,.F.);
#3733=ORIENTED_EDGE('',*,*,#2960,.F.);
#3734=ORIENTED_EDGE('',*,*,#2956,.T.);
#3735=ORIENTED_EDGE('',*,*,#2955,.T.);
#3736=ORIENTED_EDGE('',*,*,#2972,.F.);
#3737=ORIENTED_EDGE('',*,*,#2973,.T.);
#3738=ORIENTED_EDGE('',*,*,#2969,.T.);
#3739=ORIENTED_EDGE('',*,*,#2954,.T.);
#3740=ORIENTED_EDGE('',*,*,#2967,.F.);
#3741=ORIENTED_EDGE('',*,*,#2974,.T.);
#3742=ORIENTED_EDGE('',*,*,#2972,.T.);
#3743=ORIENTED_EDGE('',*,*,#2971,.T.);
#3744=ORIENTED_EDGE('',*,*,#2968,.T.);
#3745=ORIENTED_EDGE('',*,*,#2963,.T.);
#3746=ORIENTED_EDGE('',*,*,#2961,.T.);
#3747=ORIENTED_EDGE('',*,*,#2970,.F.);
#3748=ORIENTED_EDGE('',*,*,#2973,.F.);
#3749=ORIENTED_EDGE('',*,*,#2974,.F.);
#3750=ORIENTED_EDGE('',*,*,#2966,.F.);
#3751=ORIENTED_EDGE('',*,*,#2951,.T.);
#3752=ORIENTED_EDGE('',*,*,#2975,.F.);
#3753=ORIENTED_EDGE('',*,*,#2976,.F.);
#3754=ORIENTED_EDGE('',*,*,#2977,.T.);
#3755=ORIENTED_EDGE('',*,*,#2978,.F.);
#3756=ORIENTED_EDGE('',*,*,#2979,.F.);
#3757=ORIENTED_EDGE('',*,*,#2980,.T.);
#3758=ORIENTED_EDGE('',*,*,#2981,.F.);
#3759=ORIENTED_EDGE('',*,*,#2982,.F.);
#3760=ORIENTED_EDGE('',*,*,#2983,.T.);
#3761=ORIENTED_EDGE('',*,*,#2984,.F.);
#3762=ORIENTED_EDGE('',*,*,#2983,.F.);
#3763=ORIENTED_EDGE('',*,*,#2985,.F.);
#3764=ORIENTED_EDGE('',*,*,#2980,.F.);
#3765=ORIENTED_EDGE('',*,*,#2981,.T.);
#3766=ORIENTED_EDGE('',*,*,#2979,.T.);
#3767=ORIENTED_EDGE('',*,*,#2985,.T.);
#3768=ORIENTED_EDGE('',*,*,#2986,.T.);
#3769=ORIENTED_EDGE('',*,*,#2987,.T.);
#3770=ORIENTED_EDGE('',*,*,#2988,.F.);
#3771=ORIENTED_EDGE('',*,*,#2989,.T.);
#3772=ORIENTED_EDGE('',*,*,#2990,.F.);
#3773=ORIENTED_EDGE('',*,*,#2989,.F.);
#3774=ORIENTED_EDGE('',*,*,#2988,.T.);
#3775=ORIENTED_EDGE('',*,*,#2984,.T.);
#3776=ORIENTED_EDGE('',*,*,#2975,.T.);
#3777=ORIENTED_EDGE('',*,*,#2991,.F.);
#3778=ORIENTED_EDGE('',*,*,#2992,.F.);
#3779=ORIENTED_EDGE('',*,*,#2993,.F.);
#3780=ORIENTED_EDGE('',*,*,#2976,.T.);
#3781=ORIENTED_EDGE('',*,*,#2993,.T.);
#3782=ORIENTED_EDGE('',*,*,#2990,.T.);
#3783=ORIENTED_EDGE('',*,*,#2994,.F.);
#3784=ORIENTED_EDGE('',*,*,#2991,.T.);
#3785=ORIENTED_EDGE('',*,*,#2978,.T.);
#3786=ORIENTED_EDGE('',*,*,#2995,.F.);
#3787=ORIENTED_EDGE('',*,*,#2996,.T.);
#3788=ORIENTED_EDGE('',*,*,#2997,.T.);
#3789=ORIENTED_EDGE('',*,*,#2996,.F.);
#3790=ORIENTED_EDGE('',*,*,#2998,.F.);
#3791=ORIENTED_EDGE('',*,*,#2999,.T.);
#3792=ORIENTED_EDGE('',*,*,#3000,.F.);
#3793=ORIENTED_EDGE('',*,*,#2999,.F.);
#3794=ORIENTED_EDGE('',*,*,#2998,.T.);
#3795=ORIENTED_EDGE('',*,*,#3001,.F.);
#3796=ORIENTED_EDGE('',*,*,#2982,.T.);
#3797=ORIENTED_EDGE('',*,*,#2987,.F.);
#3798=ORIENTED_EDGE('',*,*,#3002,.T.);
#3799=ORIENTED_EDGE('',*,*,#3001,.T.);
#3800=ORIENTED_EDGE('',*,*,#3002,.F.);
#3801=ORIENTED_EDGE('',*,*,#2986,.F.);
#3802=ORIENTED_EDGE('',*,*,#3003,.F.);
#3803=ORIENTED_EDGE('',*,*,#3004,.T.);
#3804=ORIENTED_EDGE('',*,*,#3005,.F.);
#3805=ORIENTED_EDGE('',*,*,#3004,.F.);
#3806=ORIENTED_EDGE('',*,*,#3006,.F.);
#3807=ORIENTED_EDGE('',*,*,#3007,.T.);
#3808=ORIENTED_EDGE('',*,*,#3008,.F.);
#3809=ORIENTED_EDGE('',*,*,#3007,.F.);
#3810=ORIENTED_EDGE('',*,*,#3009,.F.);
#3811=ORIENTED_EDGE('',*,*,#3010,.T.);
#3812=ORIENTED_EDGE('',*,*,#3011,.F.);
#3813=ORIENTED_EDGE('',*,*,#3010,.F.);
#3814=ORIENTED_EDGE('',*,*,#3012,.F.);
#3815=ORIENTED_EDGE('',*,*,#3013,.T.);
#3816=ORIENTED_EDGE('',*,*,#3014,.F.);
#3817=ORIENTED_EDGE('',*,*,#3013,.F.);
#3818=ORIENTED_EDGE('',*,*,#2994,.T.);
#3819=ORIENTED_EDGE('',*,*,#2995,.T.);
#3820=ORIENTED_EDGE('',*,*,#2977,.F.);
#3821=ORIENTED_EDGE('',*,*,#2992,.T.);
#3822=ORIENTED_EDGE('',*,*,#3000,.T.);
#3823=ORIENTED_EDGE('',*,*,#3005,.T.);
#3824=ORIENTED_EDGE('',*,*,#3008,.T.);
#3825=ORIENTED_EDGE('',*,*,#3011,.T.);
#3826=ORIENTED_EDGE('',*,*,#3014,.T.);
#3827=ORIENTED_EDGE('',*,*,#2997,.F.);
#3828=ORIENTED_EDGE('',*,*,#3003,.T.);
#3829=ORIENTED_EDGE('',*,*,#3006,.T.);
#3830=ORIENTED_EDGE('',*,*,#3009,.T.);
#3831=ORIENTED_EDGE('',*,*,#3012,.T.);
#3832=ORIENTED_EDGE('',*,*,#3015,.F.);
#3833=ORIENTED_EDGE('',*,*,#3016,.T.);
#3834=ORIENTED_EDGE('',*,*,#3017,.T.);
#3835=ORIENTED_EDGE('',*,*,#3016,.F.);
#3836=ORIENTED_EDGE('',*,*,#3018,.F.);
#3837=ORIENTED_EDGE('',*,*,#3019,.T.);
#3838=ORIENTED_EDGE('',*,*,#3020,.T.);
#3839=ORIENTED_EDGE('',*,*,#3019,.F.);
#3840=ORIENTED_EDGE('',*,*,#3018,.T.);
#3841=ORIENTED_EDGE('',*,*,#3015,.T.);
#3842=ORIENTED_EDGE('',*,*,#3020,.F.);
#3843=ORIENTED_EDGE('',*,*,#3017,.F.);
#3844=ORIENTED_EDGE('',*,*,#3021,.F.);
#3845=ORIENTED_EDGE('',*,*,#3022,.F.);
#3846=ORIENTED_EDGE('',*,*,#3023,.F.);
#3847=ORIENTED_EDGE('',*,*,#3024,.T.);
#3848=ORIENTED_EDGE('',*,*,#3025,.F.);
#3849=ORIENTED_EDGE('',*,*,#3026,.F.);
#3850=ORIENTED_EDGE('',*,*,#3022,.T.);
#3851=ORIENTED_EDGE('',*,*,#3027,.F.);
#3852=ORIENTED_EDGE('',*,*,#3028,.F.);
#3853=ORIENTED_EDGE('',*,*,#3024,.F.);
#3854=ORIENTED_EDGE('',*,*,#3027,.T.);
#3855=ORIENTED_EDGE('',*,*,#3021,.T.);
#3856=ORIENTED_EDGE('',*,*,#3026,.T.);
#3857=ORIENTED_EDGE('',*,*,#3029,.T.);
#3858=ORIENTED_EDGE('',*,*,#3030,.T.);
#3859=ORIENTED_EDGE('',*,*,#3025,.T.);
#3860=ORIENTED_EDGE('',*,*,#3028,.T.);
#3861=ORIENTED_EDGE('',*,*,#3030,.F.);
#3862=ORIENTED_EDGE('',*,*,#3031,.T.);
#3863=ORIENTED_EDGE('',*,*,#3032,.F.);
#3864=ORIENTED_EDGE('',*,*,#3031,.F.);
#3865=ORIENTED_EDGE('',*,*,#3029,.F.);
#3866=ORIENTED_EDGE('',*,*,#3033,.F.);
#3867=ORIENTED_EDGE('',*,*,#3034,.T.);
#3868=ORIENTED_EDGE('',*,*,#3035,.F.);
#3869=ORIENTED_EDGE('',*,*,#3034,.F.);
#3870=ORIENTED_EDGE('',*,*,#3033,.T.);
#3871=ORIENTED_EDGE('',*,*,#3032,.T.);
#3872=ORIENTED_EDGE('',*,*,#3036,.F.);
#3873=ORIENTED_EDGE('',*,*,#3037,.T.);
#3874=ORIENTED_EDGE('',*,*,#3038,.F.);
#3875=ORIENTED_EDGE('',*,*,#3037,.F.);
#3876=ORIENTED_EDGE('',*,*,#3036,.T.);
#3877=ORIENTED_EDGE('',*,*,#3035,.T.);
#3878=ORIENTED_EDGE('',*,*,#3039,.F.);
#3879=ORIENTED_EDGE('',*,*,#3040,.T.);
#3880=ORIENTED_EDGE('',*,*,#3041,.T.);
#3881=ORIENTED_EDGE('',*,*,#3040,.F.);
#3882=ORIENTED_EDGE('',*,*,#3041,.F.);
#3883=ORIENTED_EDGE('',*,*,#3042,.F.);
#3884=ORIENTED_EDGE('',*,*,#3039,.T.);
#3885=ORIENTED_EDGE('',*,*,#3043,.F.);
#3886=ORIENTED_EDGE('',*,*,#3044,.F.);
#3887=ORIENTED_EDGE('',*,*,#3045,.T.);
#3888=ORIENTED_EDGE('',*,*,#3043,.T.);
#3889=ORIENTED_EDGE('',*,*,#3045,.F.);
#3890=ORIENTED_EDGE('',*,*,#3042,.T.);
#3891=ORIENTED_EDGE('',*,*,#3046,.T.);
#3892=ORIENTED_EDGE('',*,*,#3047,.F.);
#3893=ORIENTED_EDGE('',*,*,#3046,.F.);
#3894=ORIENTED_EDGE('',*,*,#3048,.F.);
#3895=ORIENTED_EDGE('',*,*,#3049,.T.);
#3896=ORIENTED_EDGE('',*,*,#3050,.T.);
#3897=ORIENTED_EDGE('',*,*,#3049,.F.);
#3898=ORIENTED_EDGE('',*,*,#3050,.F.);
#3899=ORIENTED_EDGE('',*,*,#3051,.F.);
#3900=ORIENTED_EDGE('',*,*,#3051,.T.);
#3901=ORIENTED_EDGE('',*,*,#3052,.T.);
#3902=ORIENTED_EDGE('',*,*,#3053,.T.);
#3903=ORIENTED_EDGE('',*,*,#3052,.F.);
#3904=ORIENTED_EDGE('',*,*,#3053,.F.);
#3905=ORIENTED_EDGE('',*,*,#3023,.T.);
#3906=ORIENTED_EDGE('',*,*,#3044,.T.);
#3907=ORIENTED_EDGE('',*,*,#3054,.F.);
#3908=ORIENTED_EDGE('',*,*,#3055,.T.);
#3909=ORIENTED_EDGE('',*,*,#3056,.F.);
#3910=ORIENTED_EDGE('',*,*,#3055,.F.);
#3911=ORIENTED_EDGE('',*,*,#3057,.F.);
#3912=ORIENTED_EDGE('',*,*,#3058,.T.);
#3913=ORIENTED_EDGE('',*,*,#3059,.F.);
#3914=ORIENTED_EDGE('',*,*,#3058,.F.);
#3915=ORIENTED_EDGE('',*,*,#3060,.F.);
#3916=ORIENTED_EDGE('',*,*,#3061,.T.);
#3917=ORIENTED_EDGE('',*,*,#3062,.F.);
#3918=ORIENTED_EDGE('',*,*,#3061,.F.);
#3919=ORIENTED_EDGE('',*,*,#3063,.F.);
#3920=ORIENTED_EDGE('',*,*,#3064,.T.);
#3921=ORIENTED_EDGE('',*,*,#3065,.F.);
#3922=ORIENTED_EDGE('',*,*,#3064,.F.);
#3923=ORIENTED_EDGE('',*,*,#3066,.F.);
#3924=ORIENTED_EDGE('',*,*,#3067,.T.);
#3925=ORIENTED_EDGE('',*,*,#3068,.T.);
#3926=ORIENTED_EDGE('',*,*,#3067,.F.);
#3927=ORIENTED_EDGE('',*,*,#3038,.T.);
#3928=ORIENTED_EDGE('',*,*,#3066,.T.);
#3929=ORIENTED_EDGE('',*,*,#3047,.T.);
#3930=ORIENTED_EDGE('',*,*,#3056,.T.);
#3931=ORIENTED_EDGE('',*,*,#3059,.T.);
#3932=ORIENTED_EDGE('',*,*,#3062,.T.);
#3933=ORIENTED_EDGE('',*,*,#3065,.T.);
#3934=ORIENTED_EDGE('',*,*,#3068,.F.);
#3935=ORIENTED_EDGE('',*,*,#3048,.T.);
#3936=ORIENTED_EDGE('',*,*,#3054,.T.);
#3937=ORIENTED_EDGE('',*,*,#3057,.T.);
#3938=ORIENTED_EDGE('',*,*,#3060,.T.);
#3939=ORIENTED_EDGE('',*,*,#3063,.T.);
#3940=ORIENTED_EDGE('',*,*,#3069,.F.);
#3941=ORIENTED_EDGE('',*,*,#3070,.T.);
#3942=ORIENTED_EDGE('',*,*,#3071,.T.);
#3943=ORIENTED_EDGE('',*,*,#3070,.F.);
#3944=ORIENTED_EDGE('',*,*,#3072,.F.);
#3945=ORIENTED_EDGE('',*,*,#3073,.T.);
#3946=ORIENTED_EDGE('',*,*,#3074,.T.);
#3947=ORIENTED_EDGE('',*,*,#3073,.F.);
#3948=ORIENTED_EDGE('',*,*,#3072,.T.);
#3949=ORIENTED_EDGE('',*,*,#3069,.T.);
#3950=ORIENTED_EDGE('',*,*,#3074,.F.);
#3951=ORIENTED_EDGE('',*,*,#3071,.F.);
#3952=ORIENTED_EDGE('',*,*,#3075,.F.);
#3953=ORIENTED_EDGE('',*,*,#3076,.T.);
#3954=ORIENTED_EDGE('',*,*,#3077,.T.);
#3955=ORIENTED_EDGE('',*,*,#3076,.F.);
#3956=ORIENTED_EDGE('',*,*,#3078,.F.);
#3957=ORIENTED_EDGE('',*,*,#3079,.T.);
#3958=ORIENTED_EDGE('',*,*,#3080,.T.);
#3959=ORIENTED_EDGE('',*,*,#3079,.F.);
#3960=ORIENTED_EDGE('',*,*,#3078,.T.);
#3961=ORIENTED_EDGE('',*,*,#3075,.T.);
#3962=ORIENTED_EDGE('',*,*,#3080,.F.);
#3963=ORIENTED_EDGE('',*,*,#3077,.F.);
#3964=ORIENTED_EDGE('',*,*,#3081,.F.);
#3965=ORIENTED_EDGE('',*,*,#3082,.T.);
#3966=ORIENTED_EDGE('',*,*,#3083,.T.);
#3967=ORIENTED_EDGE('',*,*,#3082,.F.);
#3968=ORIENTED_EDGE('',*,*,#3084,.F.);
#3969=ORIENTED_EDGE('',*,*,#3085,.T.);
#3970=ORIENTED_EDGE('',*,*,#3086,.T.);
#3971=ORIENTED_EDGE('',*,*,#3085,.F.);
#3972=ORIENTED_EDGE('',*,*,#3084,.T.);
#3973=ORIENTED_EDGE('',*,*,#3081,.T.);
#3974=ORIENTED_EDGE('',*,*,#3086,.F.);
#3975=ORIENTED_EDGE('',*,*,#3083,.F.);
#3976=ORIENTED_EDGE('',*,*,#3087,.F.);
#3977=ORIENTED_EDGE('',*,*,#3088,.T.);
#3978=ORIENTED_EDGE('',*,*,#3089,.T.);
#3979=ORIENTED_EDGE('',*,*,#3088,.F.);
#3980=ORIENTED_EDGE('',*,*,#3087,.T.);
#3981=ORIENTED_EDGE('',*,*,#3089,.F.);
#3982=ORIENTED_EDGE('',*,*,#3090,.F.);
#3983=ORIENTED_EDGE('',*,*,#3091,.T.);
#3984=ORIENTED_EDGE('',*,*,#3092,.T.);
#3985=ORIENTED_EDGE('',*,*,#3091,.F.);
#3986=ORIENTED_EDGE('',*,*,#3090,.T.);
#3987=ORIENTED_EDGE('',*,*,#3092,.F.);
#3988=ORIENTED_EDGE('',*,*,#3093,.F.);
#3989=ORIENTED_EDGE('',*,*,#3094,.T.);
#3990=ORIENTED_EDGE('',*,*,#3095,.T.);
#3991=ORIENTED_EDGE('',*,*,#3094,.F.);
#3992=ORIENTED_EDGE('',*,*,#3093,.T.);
#3993=ORIENTED_EDGE('',*,*,#3095,.F.);
#3994=ORIENTED_EDGE('',*,*,#3096,.F.);
#3995=ORIENTED_EDGE('',*,*,#3097,.T.);
#3996=ORIENTED_EDGE('',*,*,#3098,.T.);
#3997=ORIENTED_EDGE('',*,*,#3097,.F.);
#3998=ORIENTED_EDGE('',*,*,#3096,.T.);
#3999=ORIENTED_EDGE('',*,*,#3098,.F.);
#4000=ORIENTED_EDGE('',*,*,#3099,.F.);
#4001=ORIENTED_EDGE('',*,*,#3100,.F.);
#4002=ORIENTED_EDGE('',*,*,#3101,.F.);
#4003=ORIENTED_EDGE('',*,*,#3102,.F.);
#4004=ORIENTED_EDGE('',*,*,#3103,.F.);
#4005=ORIENTED_EDGE('',*,*,#3102,.T.);
#4006=ORIENTED_EDGE('',*,*,#3104,.F.);
#4007=ORIENTED_EDGE('',*,*,#3105,.T.);
#4008=ORIENTED_EDGE('',*,*,#3106,.F.);
#4009=ORIENTED_EDGE('',*,*,#3105,.F.);
#4010=ORIENTED_EDGE('',*,*,#3107,.F.);
#4011=ORIENTED_EDGE('',*,*,#3108,.F.);
#4012=ORIENTED_EDGE('',*,*,#3109,.F.);
#4013=ORIENTED_EDGE('',*,*,#3108,.T.);
#4014=ORIENTED_EDGE('',*,*,#3110,.T.);
#4015=ORIENTED_EDGE('',*,*,#3100,.T.);
#4016=ORIENTED_EDGE('',*,*,#3110,.F.);
#4017=ORIENTED_EDGE('',*,*,#3107,.T.);
#4018=ORIENTED_EDGE('',*,*,#3104,.T.);
#4019=ORIENTED_EDGE('',*,*,#3101,.T.);
#4020=ORIENTED_EDGE('',*,*,#3111,.F.);
#4021=ORIENTED_EDGE('',*,*,#3112,.T.);
#4022=ORIENTED_EDGE('',*,*,#3113,.F.);
#4023=ORIENTED_EDGE('',*,*,#3114,.T.);
#4024=ORIENTED_EDGE('',*,*,#3111,.T.);
#4025=ORIENTED_EDGE('',*,*,#3114,.F.);
#4026=ORIENTED_EDGE('',*,*,#3113,.T.);
#4027=ORIENTED_EDGE('',*,*,#3115,.F.);
#4028=ORIENTED_EDGE('',*,*,#3116,.F.);
#4029=ORIENTED_EDGE('',*,*,#3117,.T.);
#4030=ORIENTED_EDGE('',*,*,#3115,.T.);
#4031=ORIENTED_EDGE('',*,*,#3117,.F.);
#4032=ORIENTED_EDGE('',*,*,#3118,.F.);
#4033=ORIENTED_EDGE('',*,*,#3116,.T.);
#4034=ORIENTED_EDGE('',*,*,#3119,.F.);
#4035=ORIENTED_EDGE('',*,*,#3120,.T.);
#4036=ORIENTED_EDGE('',*,*,#3118,.T.);
#4037=ORIENTED_EDGE('',*,*,#3120,.F.);
#4038=ORIENTED_EDGE('',*,*,#3119,.T.);
#4039=ORIENTED_EDGE('',*,*,#3121,.F.);
#4040=ORIENTED_EDGE('',*,*,#3122,.F.);
#4041=ORIENTED_EDGE('',*,*,#3123,.T.);
#4042=ORIENTED_EDGE('',*,*,#3121,.T.);
#4043=ORIENTED_EDGE('',*,*,#3123,.F.);
#4044=ORIENTED_EDGE('',*,*,#3124,.F.);
#4045=ORIENTED_EDGE('',*,*,#3122,.T.);
#4046=ORIENTED_EDGE('',*,*,#3125,.F.);
#4047=ORIENTED_EDGE('',*,*,#3126,.T.);
#4048=ORIENTED_EDGE('',*,*,#3124,.T.);
#4049=ORIENTED_EDGE('',*,*,#3126,.F.);
#4050=ORIENTED_EDGE('',*,*,#3125,.T.);
#4051=ORIENTED_EDGE('',*,*,#3127,.F.);
#4052=ORIENTED_EDGE('',*,*,#3127,.T.);
#4053=ORIENTED_EDGE('',*,*,#3128,.T.);
#4054=ORIENTED_EDGE('',*,*,#3112,.F.);
#4055=ORIENTED_EDGE('',*,*,#3128,.F.);
#4056=ORIENTED_EDGE('',*,*,#3106,.T.);
#4057=ORIENTED_EDGE('',*,*,#3109,.T.);
#4058=ORIENTED_EDGE('',*,*,#3099,.T.);
#4059=ORIENTED_EDGE('',*,*,#3103,.T.);
#4060=ORIENTED_EDGE('',*,*,#3129,.F.);
#4061=ORIENTED_EDGE('',*,*,#3130,.F.);
#4062=ORIENTED_EDGE('',*,*,#3131,.F.);
#4063=ORIENTED_EDGE('',*,*,#3132,.F.);
#4064=ORIENTED_EDGE('',*,*,#3133,.F.);
#4065=ORIENTED_EDGE('',*,*,#3132,.T.);
#4066=ORIENTED_EDGE('',*,*,#3134,.F.);
#4067=ORIENTED_EDGE('',*,*,#3135,.T.);
#4068=ORIENTED_EDGE('',*,*,#3136,.F.);
#4069=ORIENTED_EDGE('',*,*,#3135,.F.);
#4070=ORIENTED_EDGE('',*,*,#3137,.F.);
#4071=ORIENTED_EDGE('',*,*,#3138,.F.);
#4072=ORIENTED_EDGE('',*,*,#3139,.F.);
#4073=ORIENTED_EDGE('',*,*,#3138,.T.);
#4074=ORIENTED_EDGE('',*,*,#3140,.F.);
#4075=ORIENTED_EDGE('',*,*,#3130,.T.);
#4076=ORIENTED_EDGE('',*,*,#3141,.F.);
#4077=ORIENTED_EDGE('',*,*,#3142,.T.);
#4078=ORIENTED_EDGE('',*,*,#3143,.F.);
#4079=ORIENTED_EDGE('',*,*,#3144,.T.);
#4080=ORIENTED_EDGE('',*,*,#3141,.T.);
#4081=ORIENTED_EDGE('',*,*,#3144,.F.);
#4082=ORIENTED_EDGE('',*,*,#3136,.T.);
#4083=ORIENTED_EDGE('',*,*,#3139,.T.);
#4084=ORIENTED_EDGE('',*,*,#3129,.T.);
#4085=ORIENTED_EDGE('',*,*,#3133,.T.);
#4086=ORIENTED_EDGE('',*,*,#3143,.T.);
#4087=ORIENTED_EDGE('',*,*,#3145,.F.);
#4088=ORIENTED_EDGE('',*,*,#3145,.T.);
#4089=ORIENTED_EDGE('',*,*,#3146,.T.);
#4090=ORIENTED_EDGE('',*,*,#3142,.F.);
#4091=ORIENTED_EDGE('',*,*,#3146,.F.);
#4092=ORIENTED_EDGE('',*,*,#3137,.T.);
#4093=ORIENTED_EDGE('',*,*,#3134,.T.);
#4094=ORIENTED_EDGE('',*,*,#3131,.T.);
#4095=ORIENTED_EDGE('',*,*,#3140,.T.);
#4096=ORIENTED_EDGE('',*,*,#3147,.F.);
#4097=ORIENTED_EDGE('',*,*,#3148,.F.);
#4098=ORIENTED_EDGE('',*,*,#3149,.T.);
#4099=ORIENTED_EDGE('',*,*,#3147,.T.);
#4100=ORIENTED_EDGE('',*,*,#3149,.F.);
#4101=ORIENTED_EDGE('',*,*,#3150,.F.);
#4102=ORIENTED_EDGE('',*,*,#3151,.T.);
#4103=ORIENTED_EDGE('',*,*,#3148,.T.);
#4104=ORIENTED_EDGE('',*,*,#3151,.F.);
#4105=ORIENTED_EDGE('',*,*,#3152,.F.);
#4106=ORIENTED_EDGE('',*,*,#3153,.T.);
#4107=ORIENTED_EDGE('',*,*,#3150,.T.);
#4108=ORIENTED_EDGE('',*,*,#3153,.F.);
#4109=ORIENTED_EDGE('',*,*,#3152,.T.);
#4110=ORIENTED_EDGE('',*,*,#3154,.F.);
#4111=ORIENTED_EDGE('',*,*,#3155,.F.);
#4112=ORIENTED_EDGE('',*,*,#3156,.T.);
#4113=ORIENTED_EDGE('',*,*,#3154,.T.);
#4114=ORIENTED_EDGE('',*,*,#3156,.F.);
#4115=ORIENTED_EDGE('',*,*,#3157,.F.);
#4116=ORIENTED_EDGE('',*,*,#3158,.T.);
#4117=ORIENTED_EDGE('',*,*,#3155,.T.);
#4118=ORIENTED_EDGE('',*,*,#3158,.F.);
#4119=ORIENTED_EDGE('',*,*,#3159,.F.);
#4120=ORIENTED_EDGE('',*,*,#3160,.T.);
#4121=ORIENTED_EDGE('',*,*,#3157,.T.);
#4122=ORIENTED_EDGE('',*,*,#3160,.F.);
#4123=ORIENTED_EDGE('',*,*,#3159,.T.);
#4124=ORIENTED_EDGE('',*,*,#3161,.T.);
#4125=ORIENTED_EDGE('',*,*,#3162,.T.);
#4126=ORIENTED_EDGE('',*,*,#3163,.T.);
#4127=ORIENTED_EDGE('',*,*,#3164,.F.);
#4128=ORIENTED_EDGE('',*,*,#3165,.T.);
#4129=ORIENTED_EDGE('',*,*,#3166,.T.);
#4130=ORIENTED_EDGE('',*,*,#3167,.T.);
#4131=ORIENTED_EDGE('',*,*,#3162,.F.);
#4132=ORIENTED_EDGE('',*,*,#3168,.T.);
#4133=ORIENTED_EDGE('',*,*,#3169,.T.);
#4134=ORIENTED_EDGE('',*,*,#3170,.T.);
#4135=ORIENTED_EDGE('',*,*,#3166,.F.);
#4136=ORIENTED_EDGE('',*,*,#3171,.T.);
#4137=ORIENTED_EDGE('',*,*,#3172,.T.);
#4138=ORIENTED_EDGE('',*,*,#3173,.T.);
#4139=ORIENTED_EDGE('',*,*,#3169,.F.);
#4140=ORIENTED_EDGE('',*,*,#3174,.T.);
#4141=ORIENTED_EDGE('',*,*,#3175,.T.);
#4142=ORIENTED_EDGE('',*,*,#3176,.T.);
#4143=ORIENTED_EDGE('',*,*,#3172,.F.);
#4144=ORIENTED_EDGE('',*,*,#3177,.T.);
#4145=ORIENTED_EDGE('',*,*,#3164,.T.);
#4146=ORIENTED_EDGE('',*,*,#3178,.T.);
#4147=ORIENTED_EDGE('',*,*,#3175,.F.);
#4148=ORIENTED_EDGE('',*,*,#3177,.F.);
#4149=ORIENTED_EDGE('',*,*,#3174,.F.);
#4150=ORIENTED_EDGE('',*,*,#3171,.F.);
#4151=ORIENTED_EDGE('',*,*,#3168,.F.);
#4152=ORIENTED_EDGE('',*,*,#3165,.F.);
#4153=ORIENTED_EDGE('',*,*,#3161,.F.);
#4154=ORIENTED_EDGE('',*,*,#3178,.F.);
#4155=ORIENTED_EDGE('',*,*,#3163,.F.);
#4156=ORIENTED_EDGE('',*,*,#3167,.F.);
#4157=ORIENTED_EDGE('',*,*,#3170,.F.);
#4158=ORIENTED_EDGE('',*,*,#3173,.F.);
#4159=ORIENTED_EDGE('',*,*,#3176,.F.);
#4160=ORIENTED_EDGE('',*,*,#3179,.F.);
#4161=ORIENTED_EDGE('',*,*,#3180,.T.);
#4162=ORIENTED_EDGE('',*,*,#3181,.F.);
#4163=ORIENTED_EDGE('',*,*,#3180,.F.);
#4164=ORIENTED_EDGE('',*,*,#3179,.T.);
#4165=ORIENTED_EDGE('',*,*,#3182,.F.);
#4166=ORIENTED_EDGE('',*,*,#3183,.T.);
#4167=ORIENTED_EDGE('',*,*,#3184,.T.);
#4168=ORIENTED_EDGE('',*,*,#3185,.T.);
#4169=ORIENTED_EDGE('',*,*,#3186,.T.);
#4170=ORIENTED_EDGE('',*,*,#3187,.T.);
#4171=ORIENTED_EDGE('',*,*,#3188,.T.);
#4172=ORIENTED_EDGE('',*,*,#3189,.T.);
#4173=ORIENTED_EDGE('',*,*,#3190,.F.);
#4174=ORIENTED_EDGE('',*,*,#3191,.F.);
#4175=ORIENTED_EDGE('',*,*,#3192,.F.);
#4176=ORIENTED_EDGE('',*,*,#3193,.F.);
#4177=ORIENTED_EDGE('',*,*,#3194,.F.);
#4178=ORIENTED_EDGE('',*,*,#3195,.F.);
#4179=ORIENTED_EDGE('',*,*,#3196,.F.);
#4180=ORIENTED_EDGE('',*,*,#3191,.T.);
#4181=ORIENTED_EDGE('',*,*,#3197,.T.);
#4182=ORIENTED_EDGE('',*,*,#3188,.F.);
#4183=ORIENTED_EDGE('',*,*,#3198,.F.);
#4184=ORIENTED_EDGE('',*,*,#3192,.T.);
#4185=ORIENTED_EDGE('',*,*,#3198,.T.);
#4186=ORIENTED_EDGE('',*,*,#3187,.F.);
#4187=ORIENTED_EDGE('',*,*,#3199,.F.);
#4188=ORIENTED_EDGE('',*,*,#3193,.T.);
#4189=ORIENTED_EDGE('',*,*,#3199,.T.);
#4190=ORIENTED_EDGE('',*,*,#3186,.F.);
#4191=ORIENTED_EDGE('',*,*,#3200,.F.);
#4192=ORIENTED_EDGE('',*,*,#3194,.T.);
#4193=ORIENTED_EDGE('',*,*,#3200,.T.);
#4194=ORIENTED_EDGE('',*,*,#3185,.F.);
#4195=ORIENTED_EDGE('',*,*,#3201,.F.);
#4196=ORIENTED_EDGE('',*,*,#3195,.T.);
#4197=ORIENTED_EDGE('',*,*,#3201,.T.);
#4198=ORIENTED_EDGE('',*,*,#3184,.F.);
#4199=ORIENTED_EDGE('',*,*,#3202,.F.);
#4200=ORIENTED_EDGE('',*,*,#3190,.T.);
#4201=ORIENTED_EDGE('',*,*,#3202,.T.);
#4202=ORIENTED_EDGE('',*,*,#3183,.F.);
#4203=ORIENTED_EDGE('',*,*,#3197,.F.);
#4204=ORIENTED_EDGE('',*,*,#3203,.F.);
#4205=ORIENTED_EDGE('',*,*,#3181,.T.);
#4206=ORIENTED_EDGE('',*,*,#3203,.T.);
#4207=ORIENTED_EDGE('',*,*,#3204,.T.);
#4208=ORIENTED_EDGE('',*,*,#3205,.F.);
#4209=ORIENTED_EDGE('',*,*,#3204,.F.);
#4210=ORIENTED_EDGE('',*,*,#3206,.F.);
#4211=ORIENTED_EDGE('',*,*,#3205,.T.);
#4212=ORIENTED_EDGE('',*,*,#3189,.F.);
#4213=ORIENTED_EDGE('',*,*,#3207,.T.);
#4214=ORIENTED_EDGE('',*,*,#3206,.T.);
#4215=ORIENTED_EDGE('',*,*,#3207,.F.);
#4216=ORIENTED_EDGE('',*,*,#3208,.F.);
#4217=ORIENTED_EDGE('',*,*,#3209,.T.);
#4218=ORIENTED_EDGE('',*,*,#3196,.T.);
#4219=ORIENTED_EDGE('',*,*,#3209,.F.);
#4220=ORIENTED_EDGE('',*,*,#3208,.T.);
#4221=ORIENTED_EDGE('',*,*,#3210,.F.);
#4222=ORIENTED_EDGE('',*,*,#3210,.T.);
#4223=ORIENTED_EDGE('',*,*,#3211,.T.);
#4224=ORIENTED_EDGE('',*,*,#3182,.T.);
#4225=ORIENTED_EDGE('',*,*,#3211,.F.);
#4226=ORIENTED_EDGE('',*,*,#3212,.F.);
#4227=ORIENTED_EDGE('',*,*,#3213,.T.);
#4228=ORIENTED_EDGE('',*,*,#3214,.F.);
#4229=ORIENTED_EDGE('',*,*,#3215,.T.);
#4230=ORIENTED_EDGE('',*,*,#3212,.T.);
#4231=ORIENTED_EDGE('',*,*,#3215,.F.);
#4232=ORIENTED_EDGE('',*,*,#3214,.T.);
#4233=ORIENTED_EDGE('',*,*,#3216,.F.);
#4234=ORIENTED_EDGE('',*,*,#3217,.F.);
#4235=ORIENTED_EDGE('',*,*,#3218,.T.);
#4236=ORIENTED_EDGE('',*,*,#3216,.T.);
#4237=ORIENTED_EDGE('',*,*,#3218,.F.);
#4238=ORIENTED_EDGE('',*,*,#3217,.T.);
#4239=ORIENTED_EDGE('',*,*,#3219,.F.);
#4240=ORIENTED_EDGE('',*,*,#3219,.T.);
#4241=ORIENTED_EDGE('',*,*,#3220,.T.);
#4242=ORIENTED_EDGE('',*,*,#3213,.F.);
#4243=ORIENTED_EDGE('',*,*,#3220,.F.);
#4244=ORIENTED_EDGE('',*,*,#3221,.T.);
#4245=ORIENTED_EDGE('',*,*,#3222,.T.);
#4246=ORIENTED_EDGE('',*,*,#3223,.T.);
#4247=ORIENTED_EDGE('',*,*,#3222,.F.);
#4248=ORIENTED_EDGE('',*,*,#3223,.F.);
#4249=ORIENTED_EDGE('',*,*,#3224,.T.);
#4250=ORIENTED_EDGE('',*,*,#3225,.T.);
#4251=ORIENTED_EDGE('',*,*,#3224,.F.);
#4252=ORIENTED_EDGE('',*,*,#3226,.T.);
#4253=ORIENTED_EDGE('',*,*,#3221,.F.);
#4254=ORIENTED_EDGE('',*,*,#3226,.F.);
#4255=ORIENTED_EDGE('',*,*,#3227,.T.);
#4256=ORIENTED_EDGE('',*,*,#3228,.T.);
#4257=ORIENTED_EDGE('',*,*,#3227,.F.);
#4258=ORIENTED_EDGE('',*,*,#3228,.F.);
#4259=ORIENTED_EDGE('',*,*,#3225,.F.);
#4260=ORIENTED_EDGE('',*,*,#3229,.F.);
#4261=ORIENTED_EDGE('',*,*,#3230,.F.);
#4262=ORIENTED_EDGE('',*,*,#3231,.T.);
#4263=ORIENTED_EDGE('',*,*,#3232,.F.);
#4264=ORIENTED_EDGE('',*,*,#3231,.F.);
#4265=ORIENTED_EDGE('',*,*,#3233,.F.);
#4266=ORIENTED_EDGE('',*,*,#3234,.F.);
#4267=ORIENTED_EDGE('',*,*,#3235,.F.);
#4268=ORIENTED_EDGE('',*,*,#3236,.F.);
#4269=ORIENTED_EDGE('',*,*,#3237,.F.);
#4270=ORIENTED_EDGE('',*,*,#3238,.T.);
#4271=ORIENTED_EDGE('',*,*,#3239,.F.);
#4272=ORIENTED_EDGE('',*,*,#3240,.F.);
#4273=ORIENTED_EDGE('',*,*,#3241,.F.);
#4274=ORIENTED_EDGE('',*,*,#3242,.F.);
#4275=ORIENTED_EDGE('',*,*,#3243,.F.);
#4276=ORIENTED_EDGE('',*,*,#3244,.F.);
#4277=ORIENTED_EDGE('',*,*,#3238,.F.);
#4278=ORIENTED_EDGE('',*,*,#3234,.T.);
#4279=ORIENTED_EDGE('',*,*,#3245,.T.);
#4280=ORIENTED_EDGE('',*,*,#3243,.T.);
#4281=ORIENTED_EDGE('',*,*,#3246,.F.);
#4282=ORIENTED_EDGE('',*,*,#3233,.T.);
#4283=ORIENTED_EDGE('',*,*,#3247,.T.);
#4284=ORIENTED_EDGE('',*,*,#3244,.T.);
#4285=ORIENTED_EDGE('',*,*,#3245,.F.);
#4286=ORIENTED_EDGE('',*,*,#3230,.T.);
#4287=ORIENTED_EDGE('',*,*,#3248,.T.);
#4288=ORIENTED_EDGE('',*,*,#3239,.T.);
#4289=ORIENTED_EDGE('',*,*,#3247,.F.);
#4290=ORIENTED_EDGE('',*,*,#3249,.F.);
#4291=ORIENTED_EDGE('',*,*,#3250,.T.);
#4292=ORIENTED_EDGE('',*,*,#3251,.T.);
#4293=ORIENTED_EDGE('',*,*,#3250,.F.);
#4294=ORIENTED_EDGE('',*,*,#3229,.T.);
#4295=ORIENTED_EDGE('',*,*,#3252,.T.);
#4296=ORIENTED_EDGE('',*,*,#3240,.T.);
#4297=ORIENTED_EDGE('',*,*,#3248,.F.);
#4298=ORIENTED_EDGE('',*,*,#3235,.T.);
#4299=ORIENTED_EDGE('',*,*,#3246,.T.);
#4300=ORIENTED_EDGE('',*,*,#3242,.T.);
#4301=ORIENTED_EDGE('',*,*,#3253,.F.);
#4302=ORIENTED_EDGE('',*,*,#3236,.T.);
#4303=ORIENTED_EDGE('',*,*,#3253,.T.);
#4304=ORIENTED_EDGE('',*,*,#3241,.T.);
#4305=ORIENTED_EDGE('',*,*,#3252,.F.);
#4306=ORIENTED_EDGE('',*,*,#3237,.T.);
#4307=ORIENTED_EDGE('',*,*,#3249,.T.);
#4308=ORIENTED_EDGE('',*,*,#3232,.T.);
#4309=ORIENTED_EDGE('',*,*,#3251,.F.);
#4310=ORIENTED_EDGE('',*,*,#3254,.F.);
#4311=ORIENTED_EDGE('',*,*,#3255,.T.);
#4312=ORIENTED_EDGE('',*,*,#3256,.F.);
#4313=ORIENTED_EDGE('',*,*,#3255,.F.);
#4314=ORIENTED_EDGE('',*,*,#3254,.T.);
#4315=ORIENTED_EDGE('',*,*,#3257,.F.);
#4316=ORIENTED_EDGE('',*,*,#3258,.F.);
#4317=ORIENTED_EDGE('',*,*,#3259,.T.);
#4318=ORIENTED_EDGE('',*,*,#3257,.T.);
#4319=ORIENTED_EDGE('',*,*,#3259,.F.);
#4320=ORIENTED_EDGE('',*,*,#3260,.F.);
#4321=ORIENTED_EDGE('',*,*,#3261,.F.);
#4322=ORIENTED_EDGE('',*,*,#3262,.F.);
#4323=ORIENTED_EDGE('',*,*,#3263,.T.);
#4324=ORIENTED_EDGE('',*,*,#3264,.T.);
#4325=ORIENTED_EDGE('',*,*,#3262,.T.);
#4326=ORIENTED_EDGE('',*,*,#3265,.F.);
#4327=ORIENTED_EDGE('',*,*,#3266,.F.);
#4328=ORIENTED_EDGE('',*,*,#3267,.T.);
#4329=ORIENTED_EDGE('',*,*,#3266,.T.);
#4330=ORIENTED_EDGE('',*,*,#3268,.F.);
#4331=ORIENTED_EDGE('',*,*,#3269,.F.);
#4332=ORIENTED_EDGE('',*,*,#3270,.F.);
#4333=ORIENTED_EDGE('',*,*,#3271,.T.);
#4334=ORIENTED_EDGE('',*,*,#3269,.T.);
#4335=ORIENTED_EDGE('',*,*,#3272,.F.);
#4336=ORIENTED_EDGE('',*,*,#3273,.F.);
#4337=ORIENTED_EDGE('',*,*,#3272,.T.);
#4338=ORIENTED_EDGE('',*,*,#3268,.T.);
#4339=ORIENTED_EDGE('',*,*,#3265,.T.);
#4340=ORIENTED_EDGE('',*,*,#3261,.T.);
#4341=ORIENTED_EDGE('',*,*,#3274,.F.);
#4342=ORIENTED_EDGE('',*,*,#3256,.T.);
#4343=ORIENTED_EDGE('',*,*,#3270,.T.);
#4344=ORIENTED_EDGE('',*,*,#3273,.T.);
#4345=ORIENTED_EDGE('',*,*,#3275,.T.);
#4346=ORIENTED_EDGE('',*,*,#3276,.F.);
#4347=ORIENTED_EDGE('',*,*,#3277,.F.);
#4348=ORIENTED_EDGE('',*,*,#3278,.T.);
#4349=ORIENTED_EDGE('',*,*,#3274,.T.);
#4350=ORIENTED_EDGE('',*,*,#3260,.T.);
#4351=ORIENTED_EDGE('',*,*,#3279,.T.);
#4352=ORIENTED_EDGE('',*,*,#3280,.T.);
#4353=ORIENTED_EDGE('',*,*,#3281,.T.);
#4354=ORIENTED_EDGE('',*,*,#3282,.T.);
#4355=ORIENTED_EDGE('',*,*,#3283,.T.);
#4356=ORIENTED_EDGE('',*,*,#3284,.T.);
#4357=ORIENTED_EDGE('',*,*,#3285,.T.);
#4358=ORIENTED_EDGE('',*,*,#3286,.T.);
#4359=ORIENTED_EDGE('',*,*,#3287,.F.);
#4360=ORIENTED_EDGE('',*,*,#3275,.F.);
#4361=ORIENTED_EDGE('',*,*,#3288,.F.);
#4362=ORIENTED_EDGE('',*,*,#3289,.T.);
#4363=ORIENTED_EDGE('',*,*,#3290,.F.);
#4364=ORIENTED_EDGE('',*,*,#3291,.F.);
#4365=ORIENTED_EDGE('',*,*,#3292,.F.);
#4366=ORIENTED_EDGE('',*,*,#3293,.T.);
#4367=ORIENTED_EDGE('',*,*,#3294,.F.);
#4368=ORIENTED_EDGE('',*,*,#3295,.F.);
#4369=ORIENTED_EDGE('',*,*,#3293,.F.);
#4370=ORIENTED_EDGE('',*,*,#3296,.F.);
#4371=ORIENTED_EDGE('',*,*,#3289,.F.);
#4372=ORIENTED_EDGE('',*,*,#3297,.F.);
#4373=ORIENTED_EDGE('',*,*,#3291,.T.);
#4374=ORIENTED_EDGE('',*,*,#3282,.F.);
#4375=ORIENTED_EDGE('',*,*,#3298,.F.);
#4376=ORIENTED_EDGE('',*,*,#3299,.F.);
#4377=ORIENTED_EDGE('',*,*,#3300,.F.);
#4378=ORIENTED_EDGE('',*,*,#3301,.F.);
#4379=ORIENTED_EDGE('',*,*,#3302,.F.);
#4380=ORIENTED_EDGE('',*,*,#3303,.T.);
#4381=ORIENTED_EDGE('',*,*,#3300,.T.);
#4382=ORIENTED_EDGE('',*,*,#3304,.F.);
#4383=ORIENTED_EDGE('',*,*,#3305,.F.);
#4384=ORIENTED_EDGE('',*,*,#3306,.F.);
#4385=ORIENTED_EDGE('',*,*,#3298,.T.);
#4386=ORIENTED_EDGE('',*,*,#3281,.F.);
#4387=ORIENTED_EDGE('',*,*,#3307,.F.);
#4388=ORIENTED_EDGE('',*,*,#3283,.F.);
#4389=ORIENTED_EDGE('',*,*,#3301,.T.);
#4390=ORIENTED_EDGE('',*,*,#3303,.F.);
#4391=ORIENTED_EDGE('',*,*,#3296,.T.);
#4392=ORIENTED_EDGE('',*,*,#3292,.T.);
#4393=ORIENTED_EDGE('',*,*,#3297,.T.);
#4394=ORIENTED_EDGE('',*,*,#3290,.T.);
#4395=ORIENTED_EDGE('',*,*,#3288,.T.);
#4396=ORIENTED_EDGE('',*,*,#3304,.T.);
#4397=ORIENTED_EDGE('',*,*,#3299,.T.);
#4398=ORIENTED_EDGE('',*,*,#3306,.T.);
#4399=ORIENTED_EDGE('',*,*,#3308,.T.);
#4400=ORIENTED_EDGE('',*,*,#3309,.T.);
#4401=ORIENTED_EDGE('',*,*,#3277,.T.);
#4402=ORIENTED_EDGE('',*,*,#3310,.F.);
#4403=ORIENTED_EDGE('',*,*,#3311,.F.);
#4404=ORIENTED_EDGE('',*,*,#3312,.T.);
#4405=ORIENTED_EDGE('',*,*,#3313,.T.);
#4406=ORIENTED_EDGE('',*,*,#3307,.T.);
#4407=ORIENTED_EDGE('',*,*,#3280,.F.);
#4408=ORIENTED_EDGE('',*,*,#3314,.T.);
#4409=ORIENTED_EDGE('',*,*,#3284,.F.);
#4410=ORIENTED_EDGE('',*,*,#3305,.T.);
#4411=ORIENTED_EDGE('',*,*,#3313,.F.);
#4412=ORIENTED_EDGE('',*,*,#3315,.T.);
#4413=ORIENTED_EDGE('',*,*,#3308,.F.);
#4414=ORIENTED_EDGE('',*,*,#3316,.F.);
#4415=ORIENTED_EDGE('',*,*,#3314,.F.);
#4416=ORIENTED_EDGE('',*,*,#3317,.F.);
#4417=ORIENTED_EDGE('',*,*,#3315,.F.);
#4418=ORIENTED_EDGE('',*,*,#3318,.F.);
#4419=ORIENTED_EDGE('',*,*,#3319,.T.);
#4420=ORIENTED_EDGE('',*,*,#3320,.T.);
#4421=ORIENTED_EDGE('',*,*,#3319,.F.);
#4422=ORIENTED_EDGE('',*,*,#3294,.T.);
#4423=ORIENTED_EDGE('',*,*,#3295,.T.);
#4424=ORIENTED_EDGE('',*,*,#3320,.F.);
#4425=ORIENTED_EDGE('',*,*,#3302,.T.);
#4426=ORIENTED_EDGE('',*,*,#3316,.T.);
#4427=ORIENTED_EDGE('',*,*,#3318,.T.);
#4428=ORIENTED_EDGE('',*,*,#3312,.F.);
#4429=ORIENTED_EDGE('',*,*,#3321,.F.);
#4430=ORIENTED_EDGE('',*,*,#3285,.F.);
#4431=ORIENTED_EDGE('',*,*,#3278,.F.);
#4432=ORIENTED_EDGE('',*,*,#3309,.F.);
#4433=ORIENTED_EDGE('',*,*,#3317,.T.);
#4434=ORIENTED_EDGE('',*,*,#3279,.F.);
#4435=ORIENTED_EDGE('',*,*,#3263,.F.);
#4436=ORIENTED_EDGE('',*,*,#3264,.F.);
#4437=ORIENTED_EDGE('',*,*,#3267,.F.);
#4438=ORIENTED_EDGE('',*,*,#3271,.F.);
#4439=ORIENTED_EDGE('',*,*,#3258,.T.);
#4440=ORIENTED_EDGE('',*,*,#3321,.T.);
#4441=ORIENTED_EDGE('',*,*,#3311,.T.);
#4442=ORIENTED_EDGE('',*,*,#3322,.F.);
#4443=ORIENTED_EDGE('',*,*,#3286,.F.);
#4444=ORIENTED_EDGE('',*,*,#3322,.T.);
#4445=ORIENTED_EDGE('',*,*,#3310,.T.);
#4446=ORIENTED_EDGE('',*,*,#3276,.T.);
#4447=ORIENTED_EDGE('',*,*,#3287,.T.);
#4448=ORIENTED_EDGE('',*,*,#3323,.F.);
#4449=ORIENTED_EDGE('',*,*,#3324,.T.);
#4450=ORIENTED_EDGE('',*,*,#3325,.F.);
#4451=ORIENTED_EDGE('',*,*,#3324,.F.);
#4452=ORIENTED_EDGE('',*,*,#3323,.T.);
#4453=ORIENTED_EDGE('',*,*,#3326,.F.);
#4454=ORIENTED_EDGE('',*,*,#3327,.T.);
#4455=ORIENTED_EDGE('',*,*,#3328,.T.);
#4456=ORIENTED_EDGE('',*,*,#3327,.F.);
#4457=ORIENTED_EDGE('',*,*,#3328,.F.);
#4458=ORIENTED_EDGE('',*,*,#3329,.F.);
#4459=ORIENTED_EDGE('',*,*,#3330,.T.);
#4460=ORIENTED_EDGE('',*,*,#3331,.T.);
#4461=ORIENTED_EDGE('',*,*,#3330,.F.);
#4462=ORIENTED_EDGE('',*,*,#3329,.T.);
#4463=ORIENTED_EDGE('',*,*,#3325,.T.);
#4464=ORIENTED_EDGE('',*,*,#3331,.F.);
#4465=ORIENTED_EDGE('',*,*,#3326,.T.);
#4466=ORIENTED_EDGE('',*,*,#3332,.F.);
#4467=ORIENTED_EDGE('',*,*,#3333,.T.);
#4468=ORIENTED_EDGE('',*,*,#3334,.T.);
#4469=ORIENTED_EDGE('',*,*,#3333,.F.);
#4470=ORIENTED_EDGE('',*,*,#3335,.F.);
#4471=ORIENTED_EDGE('',*,*,#3334,.F.);
#4472=ORIENTED_EDGE('',*,*,#3336,.F.);
#4473=ORIENTED_EDGE('',*,*,#3332,.T.);
#4474=ORIENTED_EDGE('',*,*,#3336,.T.);
#4475=ORIENTED_EDGE('',*,*,#3337,.T.);
#4476=ORIENTED_EDGE('',*,*,#3338,.T.);
#4477=ORIENTED_EDGE('',*,*,#3337,.F.);
#4478=ORIENTED_EDGE('',*,*,#3339,.F.);
#4479=ORIENTED_EDGE('',*,*,#3340,.T.);
#4480=ORIENTED_EDGE('',*,*,#3341,.T.);
#4481=ORIENTED_EDGE('',*,*,#3340,.F.);
#4482=ORIENTED_EDGE('',*,*,#3342,.F.);
#4483=ORIENTED_EDGE('',*,*,#3343,.T.);
#4484=ORIENTED_EDGE('',*,*,#3335,.T.);
#4485=ORIENTED_EDGE('',*,*,#3343,.F.);
#4486=ORIENTED_EDGE('',*,*,#3342,.T.);
#4487=ORIENTED_EDGE('',*,*,#3339,.T.);
#4488=ORIENTED_EDGE('',*,*,#3338,.F.);
#4489=ORIENTED_EDGE('',*,*,#3341,.F.);
#4490=ORIENTED_EDGE('',*,*,#3344,.F.);
#4491=ORIENTED_EDGE('',*,*,#3345,.T.);
#4492=ORIENTED_EDGE('',*,*,#3346,.T.);
#4493=ORIENTED_EDGE('',*,*,#3345,.F.);
#4494=ORIENTED_EDGE('',*,*,#3347,.F.);
#4495=ORIENTED_EDGE('',*,*,#3348,.T.);
#4496=ORIENTED_EDGE('',*,*,#3349,.T.);
#4497=ORIENTED_EDGE('',*,*,#3348,.F.);
#4498=ORIENTED_EDGE('',*,*,#3347,.T.);
#4499=ORIENTED_EDGE('',*,*,#3344,.T.);
#4500=ORIENTED_EDGE('',*,*,#3349,.F.);
#4501=ORIENTED_EDGE('',*,*,#3346,.F.);
#4502=ORIENTED_EDGE('',*,*,#3350,.F.);
#4503=ORIENTED_EDGE('',*,*,#3351,.T.);
#4504=ORIENTED_EDGE('',*,*,#3352,.T.);
#4505=ORIENTED_EDGE('',*,*,#3353,.T.);
#4506=ORIENTED_EDGE('',*,*,#3352,.F.);
#4507=ORIENTED_EDGE('',*,*,#3350,.T.);
#4508=ORIENTED_EDGE('',*,*,#3354,.T.);
#4509=ORIENTED_EDGE('',*,*,#3351,.F.);
#4510=ORIENTED_EDGE('',*,*,#3354,.F.);
#4511=ORIENTED_EDGE('',*,*,#3353,.F.);
#4512=ORIENTED_EDGE('',*,*,#3355,.F.);
#4513=ORIENTED_EDGE('',*,*,#3356,.F.);
#4514=ORIENTED_EDGE('',*,*,#3357,.T.);
#4515=ORIENTED_EDGE('',*,*,#3358,.T.);
#4516=ORIENTED_EDGE('',*,*,#3359,.F.);
#4517=ORIENTED_EDGE('',*,*,#3360,.F.);
#4518=ORIENTED_EDGE('',*,*,#3361,.T.);
#4519=ORIENTED_EDGE('',*,*,#3362,.T.);
#4520=ORIENTED_EDGE('',*,*,#3357,.F.);
#4521=ORIENTED_EDGE('',*,*,#3363,.F.);
#4522=ORIENTED_EDGE('',*,*,#3364,.T.);
#4523=ORIENTED_EDGE('',*,*,#3365,.T.);
#4524=ORIENTED_EDGE('',*,*,#3361,.F.);
#4525=ORIENTED_EDGE('',*,*,#3366,.F.);
#4526=ORIENTED_EDGE('',*,*,#3367,.T.);
#4527=ORIENTED_EDGE('',*,*,#3368,.T.);
#4528=ORIENTED_EDGE('',*,*,#3364,.F.);
#4529=ORIENTED_EDGE('',*,*,#3369,.F.);
#4530=ORIENTED_EDGE('',*,*,#3370,.T.);
#4531=ORIENTED_EDGE('',*,*,#3371,.T.);
#4532=ORIENTED_EDGE('',*,*,#3367,.F.);
#4533=ORIENTED_EDGE('',*,*,#3372,.F.);
#4534=ORIENTED_EDGE('',*,*,#3359,.T.);
#4535=ORIENTED_EDGE('',*,*,#3373,.T.);
#4536=ORIENTED_EDGE('',*,*,#3370,.F.);
#4537=ORIENTED_EDGE('',*,*,#3373,.F.);
#4538=ORIENTED_EDGE('',*,*,#3358,.F.);
#4539=ORIENTED_EDGE('',*,*,#3362,.F.);
#4540=ORIENTED_EDGE('',*,*,#3365,.F.);
#4541=ORIENTED_EDGE('',*,*,#3368,.F.);
#4542=ORIENTED_EDGE('',*,*,#3371,.F.);
#4543=ORIENTED_EDGE('',*,*,#3374,.F.);
#4544=ORIENTED_EDGE('',*,*,#3356,.T.);
#4545=ORIENTED_EDGE('',*,*,#3372,.T.);
#4546=ORIENTED_EDGE('',*,*,#3369,.T.);
#4547=ORIENTED_EDGE('',*,*,#3366,.T.);
#4548=ORIENTED_EDGE('',*,*,#3363,.T.);
#4549=ORIENTED_EDGE('',*,*,#3360,.T.);
#4550=ORIENTED_EDGE('',*,*,#3375,.F.);
#4551=ORIENTED_EDGE('',*,*,#3376,.T.);
#4552=ORIENTED_EDGE('',*,*,#3374,.T.);
#4553=ORIENTED_EDGE('',*,*,#3376,.F.);
#4554=ORIENTED_EDGE('',*,*,#3355,.T.);
#4555=ORIENTED_EDGE('',*,*,#3377,.T.);
#4556=ORIENTED_EDGE('',*,*,#3375,.T.);
#4557=ORIENTED_EDGE('',*,*,#3377,.F.);
#4558=ORIENTED_EDGE('',*,*,#3378,.F.);
#4559=ORIENTED_EDGE('',*,*,#3379,.F.);
#4560=ORIENTED_EDGE('',*,*,#3380,.T.);
#4561=ORIENTED_EDGE('',*,*,#3378,.T.);
#4562=ORIENTED_EDGE('',*,*,#3380,.F.);
#4563=ORIENTED_EDGE('',*,*,#3381,.F.);
#4564=ORIENTED_EDGE('',*,*,#3382,.T.);
#4565=ORIENTED_EDGE('',*,*,#3379,.T.);
#4566=ORIENTED_EDGE('',*,*,#3382,.F.);
#4567=ORIENTED_EDGE('',*,*,#3383,.F.);
#4568=ORIENTED_EDGE('',*,*,#3384,.T.);
#4569=ORIENTED_EDGE('',*,*,#3381,.T.);
#4570=ORIENTED_EDGE('',*,*,#3384,.F.);
#4571=ORIENTED_EDGE('',*,*,#3383,.T.);
#4572=ORIENTED_EDGE('',*,*,#3385,.F.);
#4573=ORIENTED_EDGE('',*,*,#3386,.F.);
#4574=ORIENTED_EDGE('',*,*,#3387,.T.);
#4575=ORIENTED_EDGE('',*,*,#3385,.T.);
#4576=ORIENTED_EDGE('',*,*,#3387,.F.);
#4577=ORIENTED_EDGE('',*,*,#3388,.F.);
#4578=ORIENTED_EDGE('',*,*,#3389,.T.);
#4579=ORIENTED_EDGE('',*,*,#3386,.T.);
#4580=ORIENTED_EDGE('',*,*,#3389,.F.);
#4581=ORIENTED_EDGE('',*,*,#3390,.F.);
#4582=ORIENTED_EDGE('',*,*,#3391,.T.);
#4583=ORIENTED_EDGE('',*,*,#3388,.T.);
#4584=ORIENTED_EDGE('',*,*,#3391,.F.);
#4585=ORIENTED_EDGE('',*,*,#3390,.T.);
#4586=ORIENTED_EDGE('',*,*,#3392,.T.);
#4587=ORIENTED_EDGE('',*,*,#3393,.T.);
#4588=ORIENTED_EDGE('',*,*,#3394,.T.);
#4589=ORIENTED_EDGE('',*,*,#3395,.F.);
#4590=ORIENTED_EDGE('',*,*,#3396,.T.);
#4591=ORIENTED_EDGE('',*,*,#3397,.T.);
#4592=ORIENTED_EDGE('',*,*,#3398,.T.);
#4593=ORIENTED_EDGE('',*,*,#3393,.F.);
#4594=ORIENTED_EDGE('',*,*,#3399,.T.);
#4595=ORIENTED_EDGE('',*,*,#3400,.T.);
#4596=ORIENTED_EDGE('',*,*,#3401,.T.);
#4597=ORIENTED_EDGE('',*,*,#3397,.F.);
#4598=ORIENTED_EDGE('',*,*,#3402,.T.);
#4599=ORIENTED_EDGE('',*,*,#3403,.T.);
#4600=ORIENTED_EDGE('',*,*,#3404,.T.);
#4601=ORIENTED_EDGE('',*,*,#3400,.F.);
#4602=ORIENTED_EDGE('',*,*,#3405,.T.);
#4603=ORIENTED_EDGE('',*,*,#3406,.T.);
#4604=ORIENTED_EDGE('',*,*,#3407,.T.);
#4605=ORIENTED_EDGE('',*,*,#3403,.F.);
#4606=ORIENTED_EDGE('',*,*,#3408,.T.);
#4607=ORIENTED_EDGE('',*,*,#3395,.T.);
#4608=ORIENTED_EDGE('',*,*,#3409,.T.);
#4609=ORIENTED_EDGE('',*,*,#3406,.F.);
#4610=ORIENTED_EDGE('',*,*,#3408,.F.);
#4611=ORIENTED_EDGE('',*,*,#3405,.F.);
#4612=ORIENTED_EDGE('',*,*,#3402,.F.);
#4613=ORIENTED_EDGE('',*,*,#3399,.F.);
#4614=ORIENTED_EDGE('',*,*,#3396,.F.);
#4615=ORIENTED_EDGE('',*,*,#3392,.F.);
#4616=ORIENTED_EDGE('',*,*,#3409,.F.);
#4617=ORIENTED_EDGE('',*,*,#3394,.F.);
#4618=ORIENTED_EDGE('',*,*,#3398,.F.);
#4619=ORIENTED_EDGE('',*,*,#3401,.F.);
#4620=ORIENTED_EDGE('',*,*,#3404,.F.);
#4621=ORIENTED_EDGE('',*,*,#3407,.F.);
#4622=CYLINDRICAL_SURFACE('',#5435,0.275);
#4623=CYLINDRICAL_SURFACE('',#5438,0.275);
#4624=CYLINDRICAL_SURFACE('',#5441,0.275);
#4625=CYLINDRICAL_SURFACE('',#5444,0.275);
#4626=CYLINDRICAL_SURFACE('',#5447,0.275);
#4627=CYLINDRICAL_SURFACE('',#5450,0.275);
#4628=CYLINDRICAL_SURFACE('',#5453,0.275);
#4629=CYLINDRICAL_SURFACE('',#5456,0.275);
#4630=CYLINDRICAL_SURFACE('',#5459,0.275);
#4631=CYLINDRICAL_SURFACE('',#5483,0.165);
#4632=CYLINDRICAL_SURFACE('',#5487,0.165);
#4633=CYLINDRICAL_SURFACE('',#5491,0.165);
#4634=CYLINDRICAL_SURFACE('',#5495,0.165);
#4635=CYLINDRICAL_SURFACE('',#5499,0.21);
#4636=CYLINDRICAL_SURFACE('',#5503,0.21);
#4637=CYLINDRICAL_SURFACE('',#5507,0.21);
#4638=CYLINDRICAL_SURFACE('',#5511,0.21);
#4639=CYLINDRICAL_SURFACE('',#5515,1.05);
#4640=CYLINDRICAL_SURFACE('',#5520,0.625);
#4641=CYLINDRICAL_SURFACE('',#5529,0.375);
#4642=CYLINDRICAL_SURFACE('',#5534,0.375);
#4643=CYLINDRICAL_SURFACE('',#5539,0.375);
#4644=CYLINDRICAL_SURFACE('',#5544,0.375);
#4645=CYLINDRICAL_SURFACE('',#5549,0.225);
#4646=CYLINDRICAL_SURFACE('',#5551,0.225);
#4647=CYLINDRICAL_SURFACE('',#5553,0.225);
#4648=CYLINDRICAL_SURFACE('',#5555,0.225);
#4649=CYLINDRICAL_SURFACE('',#5557,1.04);
#4650=CYLINDRICAL_SURFACE('',#5562,0.625);
#4651=CYLINDRICAL_SURFACE('',#5564,2.);
#4652=CYLINDRICAL_SURFACE('',#5570,0.625);
#4653=CYLINDRICAL_SURFACE('',#5573,0.8);
#4654=CYLINDRICAL_SURFACE('',#5584,0.21);
#4655=CYLINDRICAL_SURFACE('',#5598,0.8);
#4656=CYLINDRICAL_SURFACE('',#5602,0.2);
#4657=CYLINDRICAL_SURFACE('',#5607,0.515);
#4658=CYLINDRICAL_SURFACE('',#5611,0.8);
#4659=CYLINDRICAL_SURFACE('',#5614,2.4);
#4660=CYLINDRICAL_SURFACE('',#5618,1.25);
#4661=CYLINDRICAL_SURFACE('',#5623,1.);
#4662=CYLINDRICAL_SURFACE('',#5624,0.275);
#4663=CYLINDRICAL_SURFACE('',#5627,0.275);
#4664=CYLINDRICAL_SURFACE('',#5630,0.275);
#4665=CYLINDRICAL_SURFACE('',#5633,0.275);
#4666=CYLINDRICAL_SURFACE('',#5639,1.);
#4667=CYLINDRICAL_SURFACE('',#5642,1.25);
#4668=CYLINDRICAL_SURFACE('',#5650,0.15);
#4669=CYLINDRICAL_SURFACE('',#5655,0.2);
#4670=CYLINDRICAL_SURFACE('',#5657,0.515);
#4671=CYLINDRICAL_SURFACE('',#5661,0.8);
#4672=CYLINDRICAL_SURFACE('',#5664,0.5);
#4673=CYLINDRICAL_SURFACE('',#5671,0.41);
#4674=CYLINDRICAL_SURFACE('',#5673,0.41);
#4675=CYLINDRICAL_SURFACE('',#5675,1.25);
#4676=CYLINDRICAL_SURFACE('',#5680,1.);
#4677=CYLINDRICAL_SURFACE('',#5683,0.275);
#4678=CYLINDRICAL_SURFACE('',#5686,0.275);
#4679=CYLINDRICAL_SURFACE('',#5689,0.275);
#4680=CYLINDRICAL_SURFACE('',#5692,0.275);
#4681=CYLINDRICAL_SURFACE('',#5695,2.4);
#4682=CYLINDRICAL_SURFACE('',#5701,1.);
#4683=CYLINDRICAL_SURFACE('',#5704,1.25);
#4684=CYLINDRICAL_SURFACE('',#5710,1.);
#4685=CYLINDRICAL_SURFACE('',#5713,1.25);
#4686=CYLINDRICAL_SURFACE('',#5719,0.4);
#4687=CYLINDRICAL_SURFACE('',#5722,0.5);
#4688=CYLINDRICAL_SURFACE('',#5728,0.25);
#4689=CYLINDRICAL_SURFACE('',#5734,0.25);
#4690=CYLINDRICAL_SURFACE('',#5740,0.25);
#4691=CYLINDRICAL_SURFACE('',#5746,0.25);
#4692=CYLINDRICAL_SURFACE('',#5763,1.05);
#4693=CYLINDRICAL_SURFACE('',#5767,1.);
#4694=CYLINDRICAL_SURFACE('',#5771,1.05);
#4695=CYLINDRICAL_SURFACE('',#5775,1.);
#4696=CYLINDRICAL_SURFACE('',#5779,1.05);
#4697=CYLINDRICAL_SURFACE('',#5783,0.9);
#4698=CYLINDRICAL_SURFACE('',#5796,0.895);
#4699=CYLINDRICAL_SURFACE('',#5800,0.605);
#4700=CYLINDRICAL_SURFACE('',#5808,0.425);
#4701=CYLINDRICAL_SURFACE('',#5816,0.24505);
#4702=CYLINDRICAL_SURFACE('',#5831,0.43);
#4703=CYLINDRICAL_SURFACE('',#5848,0.46);
#4704=CYLINDRICAL_SURFACE('',#5852,0.525);
#4705=CYLINDRICAL_SURFACE('',#5853,0.515);
#4706=CYLINDRICAL_SURFACE('',#5857,0.2);
#4707=CYLINDRICAL_SURFACE('',#5862,0.475);
#4708=CYLINDRICAL_SURFACE('',#5866,0.355);
#4709=CYLINDRICAL_SURFACE('',#5870,0.31);
#4710=CYLINDRICAL_SURFACE('',#5877,0.265);
#4711=CYLINDRICAL_SURFACE('',#5881,0.5);
#4712=CYLINDRICAL_SURFACE('',#5892,0.2117);
#4713=CYLINDRICAL_SURFACE('',#5902,0.4);
#4714=CYLINDRICAL_SURFACE('',#5907,0.225);
#4715=CYLINDRICAL_SURFACE('',#5918,0.164999999999999);
#4716=CYLINDRICAL_SURFACE('',#5925,0.605);
#4717=CYLINDRICAL_SURFACE('',#5934,1.);
#4718=CYLINDRICAL_SURFACE('',#5945,0.165);
#4719=CYLINDRICAL_SURFACE('',#5949,0.165);
#4720=CYLINDRICAL_SURFACE('',#5953,0.4);
#4721=CYLINDRICAL_SURFACE('',#5959,0.94);
#4722=CYLINDRICAL_SURFACE('',#5966,0.99);
#4723=CYLINDRICAL_SURFACE('',#5968,0.225);
#4724=CYLINDRICAL_SURFACE('',#5971,0.99);
#4725=CYLINDRICAL_SURFACE('',#5976,0.94);
#4726=CYLINDRICAL_SURFACE('',#5979,1.);
#4727=CYLINDRICAL_SURFACE('',#5990,0.6);
#4728=CYLINDRICAL_SURFACE('',#6006,0.1954);
#4729=CYLINDRICAL_SURFACE('',#6012,0.35);
#4730=CYLINDRICAL_SURFACE('',#6020,0.1954);
#4731=ADVANCED_FACE('',(#736),#4622,.F.);
#4732=ADVANCED_FACE('',(#737),#4623,.F.);
#4733=ADVANCED_FACE('',(#738),#4624,.F.);
#4734=ADVANCED_FACE('',(#739),#4625,.F.);
#4735=ADVANCED_FACE('',(#740),#4626,.F.);
#4736=ADVANCED_FACE('',(#741),#4627,.F.);
#4737=ADVANCED_FACE('',(#742),#4628,.F.);
#4738=ADVANCED_FACE('',(#743),#4629,.F.);
#4739=ADVANCED_FACE('',(#744),#4630,.F.);
#4740=ADVANCED_FACE('',(#745),#545,.T.);
#4741=ADVANCED_FACE('',(#746),#546,.T.);
#4742=ADVANCED_FACE('',(#747),#547,.T.);
#4743=ADVANCED_FACE('',(#748),#548,.T.);
#4744=ADVANCED_FACE('',(#749,#419,#420,#421,#422,#423,#424,#425,#426,#427),
#549,.T.);
#4745=ADVANCED_FACE('',(#750,#428,#429,#430,#431,#432,#433,#434,#435,#436),
#550,.F.);
#4746=ADVANCED_FACE('',(#751),#551,.T.);
#4747=ADVANCED_FACE('',(#752),#552,.T.);
#4748=ADVANCED_FACE('',(#753),#553,.T.);
#4749=ADVANCED_FACE('',(#754),#554,.T.);
#4750=ADVANCED_FACE('',(#755),#555,.T.);
#4751=ADVANCED_FACE('',(#756),#556,.F.);
#4752=ADVANCED_FACE('',(#757),#557,.T.);
#4753=ADVANCED_FACE('',(#758),#558,.T.);
#4754=ADVANCED_FACE('',(#759),#559,.T.);
#4755=ADVANCED_FACE('',(#760),#560,.T.);
#4756=ADVANCED_FACE('',(#761),#561,.T.);
#4757=ADVANCED_FACE('',(#762),#562,.F.);
#4758=ADVANCED_FACE('',(#763),#4631,.F.);
#4759=ADVANCED_FACE('',(#764),#563,.T.);
#4760=ADVANCED_FACE('',(#765),#4632,.F.);
#4761=ADVANCED_FACE('',(#766),#564,.T.);
#4762=ADVANCED_FACE('',(#767),#4633,.F.);
#4763=ADVANCED_FACE('',(#768),#565,.T.);
#4764=ADVANCED_FACE('',(#769),#4634,.F.);
#4765=ADVANCED_FACE('',(#770),#566,.T.);
#4766=ADVANCED_FACE('',(#771),#4635,.F.);
#4767=ADVANCED_FACE('',(#772),#567,.F.);
#4768=ADVANCED_FACE('',(#773),#4636,.F.);
#4769=ADVANCED_FACE('',(#774),#568,.F.);
#4770=ADVANCED_FACE('',(#775),#4637,.F.);
#4771=ADVANCED_FACE('',(#776),#569,.F.);
#4772=ADVANCED_FACE('',(#777),#4638,.F.);
#4773=ADVANCED_FACE('',(#778),#570,.F.);
#4774=ADVANCED_FACE('',(#779),#4639,.F.);
#4775=ADVANCED_FACE('',(#780,#437),#571,.T.);
#4776=ADVANCED_FACE('',(#781),#4640,.F.);
#4777=ADVANCED_FACE('',(#782),#572,.T.);
#4778=ADVANCED_FACE('',(#783),#573,.T.);
#4779=ADVANCED_FACE('',(#784),#574,.T.);
#4780=ADVANCED_FACE('',(#785),#575,.T.);
#4781=ADVANCED_FACE('',(#786,#438,#439,#440,#441,#442),#576,.T.);
#4782=ADVANCED_FACE('',(#787,#443,#444,#445,#446,#447),#577,.F.);
#4783=ADVANCED_FACE('',(#788),#4641,.F.);
#4784=ADVANCED_FACE('',(#789,#448),#578,.T.);
#4785=ADVANCED_FACE('',(#790),#4642,.F.);
#4786=ADVANCED_FACE('',(#791,#449),#579,.T.);
#4787=ADVANCED_FACE('',(#792),#4643,.F.);
#4788=ADVANCED_FACE('',(#793,#450),#580,.T.);
#4789=ADVANCED_FACE('',(#794),#4644,.F.);
#4790=ADVANCED_FACE('',(#795,#451),#581,.T.);
#4791=ADVANCED_FACE('',(#796),#4645,.F.);
#4792=ADVANCED_FACE('',(#797),#4646,.F.);
#4793=ADVANCED_FACE('',(#798),#4647,.F.);
#4794=ADVANCED_FACE('',(#799),#4648,.F.);
#4795=ADVANCED_FACE('',(#800),#4649,.T.);
#4796=ADVANCED_FACE('',(#801,#452),#582,.F.);
#4797=ADVANCED_FACE('',(#802),#4650,.F.);
#4798=ADVANCED_FACE('',(#803),#4651,.T.);
#4799=ADVANCED_FACE('',(#804,#453,#454,#455,#456,#457),#583,.T.);
#4800=ADVANCED_FACE('',(#805,#458,#459,#460,#461,#462),#584,.F.);
#4801=ADVANCED_FACE('',(#806),#4652,.F.);
#4802=ADVANCED_FACE('',(#807),#4653,.T.);
#4803=ADVANCED_FACE('',(#808,#463),#585,.T.);
#4804=ADVANCED_FACE('',(#809,#464),#586,.F.);
#4805=ADVANCED_FACE('',(#810),#292,.T.);
#4806=ADVANCED_FACE('',(#811),#587,.T.);
#4807=ADVANCED_FACE('',(#812),#588,.F.);
#4808=ADVANCED_FACE('',(#813),#4654,.F.);
#4809=ADVANCED_FACE('',(#814),#589,.F.);
#4810=ADVANCED_FACE('',(#815),#590,.F.);
#4811=ADVANCED_FACE('',(#816),#591,.T.);
#4812=ADVANCED_FACE('',(#817),#592,.T.);
#4813=ADVANCED_FACE('',(#818),#593,.T.);
#4814=ADVANCED_FACE('',(#819),#594,.T.);
#4815=ADVANCED_FACE('',(#820),#595,.T.);
#4816=ADVANCED_FACE('',(#821),#596,.T.);
#4817=ADVANCED_FACE('',(#822),#597,.T.);
#4818=ADVANCED_FACE('',(#823,#465),#598,.F.);
#4819=ADVANCED_FACE('',(#824),#4655,.F.);
#4820=ADVANCED_FACE('',(#825),#599,.T.);
#4821=ADVANCED_FACE('',(#826),#4656,.F.);
#4822=ADVANCED_FACE('',(#827),#600,.T.);
#4823=ADVANCED_FACE('',(#828),#4657,.F.);
#4824=ADVANCED_FACE('',(#829,#466),#601,.T.);
#4825=ADVANCED_FACE('',(#830),#4658,.F.);
#4826=ADVANCED_FACE('',(#831,#467),#602,.T.);
#4827=ADVANCED_FACE('',(#832),#4659,.T.);
#4828=ADVANCED_FACE('',(#833),#4660,.F.);
#4829=ADVANCED_FACE('',(#834,#468),#603,.T.);
#4830=ADVANCED_FACE('',(#835),#4661,.F.);
#4831=ADVANCED_FACE('',(#836),#4662,.F.);
#4832=ADVANCED_FACE('',(#837),#4663,.F.);
#4833=ADVANCED_FACE('',(#838),#4664,.F.);
#4834=ADVANCED_FACE('',(#839),#4665,.F.);
#4835=ADVANCED_FACE('',(#840,#469,#470,#471,#472,#473),#604,.T.);
#4836=ADVANCED_FACE('',(#841,#474,#475,#476,#477),#605,.F.);
#4837=ADVANCED_FACE('',(#842),#4666,.F.);
#4838=ADVANCED_FACE('',(#843),#4667,.T.);
#4839=ADVANCED_FACE('',(#844,#478),#606,.T.);
#4840=ADVANCED_FACE('',(#845,#479),#607,.F.);
#4841=ADVANCED_FACE('',(#846),#608,.F.);
#4842=ADVANCED_FACE('',(#847),#4668,.F.);
#4843=ADVANCED_FACE('',(#848),#609,.T.);
#4844=ADVANCED_FACE('',(#849),#4669,.F.);
#4845=ADVANCED_FACE('',(#850),#4670,.F.);
#4846=ADVANCED_FACE('',(#851,#480),#610,.T.);
#4847=ADVANCED_FACE('',(#852),#4671,.F.);
#4848=ADVANCED_FACE('',(#853,#481),#611,.T.);
#4849=ADVANCED_FACE('',(#854),#4672,.F.);
#4850=ADVANCED_FACE('',(#855,#482),#612,.F.);
#4851=ADVANCED_FACE('',(#856,#483),#613,.T.);
#4852=ADVANCED_FACE('',(#857),#4673,.F.);
#4853=ADVANCED_FACE('',(#858),#4674,.F.);
#4854=ADVANCED_FACE('',(#859),#4675,.F.);
#4855=ADVANCED_FACE('',(#860,#484),#614,.F.);
#4856=ADVANCED_FACE('',(#861),#4676,.F.);
#4857=ADVANCED_FACE('',(#862,#485,#486),#615,.F.);
#4858=ADVANCED_FACE('',(#863),#4677,.F.);
#4859=ADVANCED_FACE('',(#864),#4678,.F.);
#4860=ADVANCED_FACE('',(#865),#4679,.F.);
#4861=ADVANCED_FACE('',(#866),#4680,.F.);
#4862=ADVANCED_FACE('',(#867,#487),#4681,.T.);
#4863=ADVANCED_FACE('',(#868,#488,#489,#490,#491,#492),#616,.T.);
#4864=ADVANCED_FACE('',(#869,#493,#494,#495,#496,#497),#617,.F.);
#4865=ADVANCED_FACE('',(#870),#4682,.F.);
#4866=ADVANCED_FACE('',(#871),#4683,.T.);
#4867=ADVANCED_FACE('',(#872,#498),#618,.T.);
#4868=ADVANCED_FACE('',(#873,#499),#619,.F.);
#4869=ADVANCED_FACE('',(#874),#4684,.F.);
#4870=ADVANCED_FACE('',(#875),#4685,.T.);
#4871=ADVANCED_FACE('',(#876,#500),#620,.T.);
#4872=ADVANCED_FACE('',(#877,#501),#621,.F.);
#4873=ADVANCED_FACE('',(#878),#4686,.F.);
#4874=ADVANCED_FACE('',(#879),#4687,.T.);
#4875=ADVANCED_FACE('',(#880,#502),#622,.T.);
#4876=ADVANCED_FACE('',(#881,#503),#623,.F.);
#4877=ADVANCED_FACE('',(#882),#4688,.T.);
#4878=ADVANCED_FACE('',(#883),#624,.T.);
#4879=ADVANCED_FACE('',(#884),#625,.F.);
#4880=ADVANCED_FACE('',(#885),#4689,.T.);
#4881=ADVANCED_FACE('',(#886),#626,.T.);
#4882=ADVANCED_FACE('',(#887),#627,.F.);
#4883=ADVANCED_FACE('',(#888),#4690,.T.);
#4884=ADVANCED_FACE('',(#889),#628,.T.);
#4885=ADVANCED_FACE('',(#890),#629,.F.);
#4886=ADVANCED_FACE('',(#891),#4691,.T.);
#4887=ADVANCED_FACE('',(#892),#630,.T.);
#4888=ADVANCED_FACE('',(#893),#631,.F.);
#4889=ADVANCED_FACE('',(#894),#632,.F.);
#4890=ADVANCED_FACE('',(#895),#633,.F.);
#4891=ADVANCED_FACE('',(#896),#634,.F.);
#4892=ADVANCED_FACE('',(#897),#635,.F.);
#4893=ADVANCED_FACE('',(#898),#636,.F.);
#4894=ADVANCED_FACE('',(#899,#504),#637,.T.);
#4895=ADVANCED_FACE('',(#900),#4692,.T.);
#4896=ADVANCED_FACE('',(#901,#505),#638,.T.);
#4897=ADVANCED_FACE('',(#902),#4693,.T.);
#4898=ADVANCED_FACE('',(#903,#506),#639,.T.);
#4899=ADVANCED_FACE('',(#904),#4694,.T.);
#4900=ADVANCED_FACE('',(#905,#507),#640,.T.);
#4901=ADVANCED_FACE('',(#906),#4695,.T.);
#4902=ADVANCED_FACE('',(#907,#508),#641,.T.);
#4903=ADVANCED_FACE('',(#908),#4696,.T.);
#4904=ADVANCED_FACE('',(#909,#509),#642,.T.);
#4905=ADVANCED_FACE('',(#910,#510),#4697,.F.);
#4906=ADVANCED_FACE('',(#911),#643,.F.);
#4907=ADVANCED_FACE('',(#912),#644,.F.);
#4908=ADVANCED_FACE('',(#913),#645,.F.);
#4909=ADVANCED_FACE('',(#914),#646,.F.);
#4910=ADVANCED_FACE('',(#915,#511),#647,.T.);
#4911=ADVANCED_FACE('',(#916,#512),#4698,.T.);
#4912=ADVANCED_FACE('',(#917,#513),#648,.T.);
#4913=ADVANCED_FACE('',(#918,#514),#4699,.F.);
#4914=ADVANCED_FACE('',(#919),#649,.T.);
#4915=ADVANCED_FACE('',(#920),#25,.T.);
#4916=ADVANCED_FACE('',(#921),#4700,.T.);
#4917=ADVANCED_FACE('',(#922),#26,.T.);
#4918=ADVANCED_FACE('',(#923,#515),#650,.T.);
#4919=ADVANCED_FACE('',(#924),#27,.T.);
#4920=ADVANCED_FACE('',(#925),#4701,.T.);
#4921=ADVANCED_FACE('',(#926),#28,.T.);
#4922=ADVANCED_FACE('',(#927),#651,.T.);
#4923=ADVANCED_FACE('',(#928),#652,.F.);
#4924=ADVANCED_FACE('',(#929),#653,.F.);
#4925=ADVANCED_FACE('',(#930),#654,.F.);
#4926=ADVANCED_FACE('',(#931),#655,.F.);
#4927=ADVANCED_FACE('',(#932),#656,.F.);
#4928=ADVANCED_FACE('',(#933),#657,.F.);
#4929=ADVANCED_FACE('',(#934),#658,.F.);
#4930=ADVANCED_FACE('',(#935),#659,.F.);
#4931=ADVANCED_FACE('',(#936),#4702,.F.);
#4932=ADVANCED_FACE('',(#937,#516),#660,.T.);
#4933=ADVANCED_FACE('',(#938,#517),#661,.T.);
#4934=ADVANCED_FACE('',(#939,#518),#662,.F.);
#4935=ADVANCED_FACE('',(#940),#663,.T.);
#4936=ADVANCED_FACE('',(#941),#664,.T.);
#4937=ADVANCED_FACE('',(#942),#665,.T.);
#4938=ADVANCED_FACE('',(#943),#666,.T.);
#4939=ADVANCED_FACE('',(#944),#667,.T.);
#4940=ADVANCED_FACE('',(#945),#668,.T.);
#4941=ADVANCED_FACE('',(#946,#519),#669,.T.);
#4942=ADVANCED_FACE('',(#947),#4703,.F.);
#4943=ADVANCED_FACE('',(#948,#520),#670,.T.);
#4944=ADVANCED_FACE('',(#949),#4704,.T.);
#4945=ADVANCED_FACE('',(#950),#4705,.T.);
#4946=ADVANCED_FACE('',(#951,#521),#671,.T.);
#4947=ADVANCED_FACE('',(#952),#4706,.F.);
#4948=ADVANCED_FACE('',(#953,#522),#672,.T.);
#4949=ADVANCED_FACE('',(#954),#4707,.T.);
#4950=ADVANCED_FACE('',(#955,#523),#673,.T.);
#4951=ADVANCED_FACE('',(#956),#4708,.T.);
#4952=ADVANCED_FACE('',(#957,#524),#674,.T.);
#4953=ADVANCED_FACE('',(#958),#4709,.F.);
#4954=ADVANCED_FACE('',(#959),#29,.F.);
#4955=ADVANCED_FACE('',(#960),#4710,.F.);
#4956=ADVANCED_FACE('',(#961,#525),#675,.T.);
#4957=ADVANCED_FACE('',(#962),#4711,.T.);
#4958=ADVANCED_FACE('',(#963,#526),#676,.F.);
#4959=ADVANCED_FACE('',(#964),#30,.T.);
#4960=ADVANCED_FACE('',(#965),#31,.T.);
#4961=ADVANCED_FACE('',(#966),#677,.T.);
#4962=ADVANCED_FACE('',(#967),#678,.T.);
#4963=ADVANCED_FACE('',(#968),#679,.T.);
#4964=ADVANCED_FACE('',(#969),#4712,.F.);
#4965=ADVANCED_FACE('',(#970),#680,.T.);
#4966=ADVANCED_FACE('',(#971),#681,.T.);
#4967=ADVANCED_FACE('',(#972),#682,.T.);
#4968=ADVANCED_FACE('',(#973,#527),#683,.T.);
#4969=ADVANCED_FACE('',(#974,#528),#684,.F.);
#4970=ADVANCED_FACE('',(#975),#4713,.F.);
#4971=ADVANCED_FACE('',(#976,#529),#685,.T.);
#4972=ADVANCED_FACE('',(#977),#4714,.F.);
#4973=ADVANCED_FACE('',(#978),#686,.T.);
#4974=ADVANCED_FACE('',(#979),#687,.T.);
#4975=ADVANCED_FACE('',(#980),#688,.T.);
#4976=ADVANCED_FACE('',(#981),#689,.T.);
#4977=ADVANCED_FACE('',(#982,#530),#690,.T.);
#4978=ADVANCED_FACE('',(#983),#691,.T.);
#4979=ADVANCED_FACE('',(#984),#692,.T.);
#4980=ADVANCED_FACE('',(#985),#693,.T.);
#4981=ADVANCED_FACE('',(#986),#4715,.F.);
#4982=ADVANCED_FACE('',(#987),#694,.T.);
#4983=ADVANCED_FACE('',(#988),#695,.F.);
#4984=ADVANCED_FACE('',(#989,#531),#4716,.F.);
#4985=ADVANCED_FACE('',(#990),#696,.T.);
#4986=ADVANCED_FACE('',(#991),#697,.T.);
#4987=ADVANCED_FACE('',(#992),#698,.T.);
#4988=ADVANCED_FACE('',(#993,#532),#4717,.T.);
#4989=ADVANCED_FACE('',(#994,#533),#699,.F.);
#4990=ADVANCED_FACE('',(#995),#700,.F.);
#4991=ADVANCED_FACE('',(#996,#534),#701,.F.);
#4992=ADVANCED_FACE('',(#997),#702,.T.);
#4993=ADVANCED_FACE('',(#998),#703,.T.);
#4994=ADVANCED_FACE('',(#999),#4718,.F.);
#4995=ADVANCED_FACE('',(#1000),#704,.T.);
#4996=ADVANCED_FACE('',(#1001),#4719,.F.);
#4997=ADVANCED_FACE('',(#1002),#705,.F.);
#4998=ADVANCED_FACE('',(#1003),#4720,.T.);
#4999=ADVANCED_FACE('',(#1004,#535),#706,.T.);
#5000=ADVANCED_FACE('',(#1005,#536),#707,.F.);
#5001=ADVANCED_FACE('',(#1006),#4721,.T.);
#5002=ADVANCED_FACE('',(#1007,#537),#708,.F.);
#5003=ADVANCED_FACE('',(#1008,#538),#709,.T.);
#5004=ADVANCED_FACE('',(#1009),#4722,.T.);
#5005=ADVANCED_FACE('',(#1010),#4723,.F.);
#5006=ADVANCED_FACE('',(#1011),#4724,.T.);
#5007=ADVANCED_FACE('',(#1012,#539),#710,.T.);
#5008=ADVANCED_FACE('',(#1013,#540),#711,.F.);
#5009=ADVANCED_FACE('',(#1014),#4725,.F.);
#5010=ADVANCED_FACE('',(#1015),#4726,.T.);
#5011=ADVANCED_FACE('',(#1016,#541),#712,.T.);
#5012=ADVANCED_FACE('',(#1017,#542),#713,.F.);
#5013=ADVANCED_FACE('',(#1018),#714,.T.);
#5014=ADVANCED_FACE('',(#1019),#32,.T.);
#5015=ADVANCED_FACE('',(#1020),#4727,.T.);
#5016=ADVANCED_FACE('',(#1021),#715,.F.);
#5017=ADVANCED_FACE('',(#1022),#716,.F.);
#5018=ADVANCED_FACE('',(#1023),#717,.F.);
#5019=ADVANCED_FACE('',(#1024),#718,.F.);
#5020=ADVANCED_FACE('',(#1025),#719,.F.);
#5021=ADVANCED_FACE('',(#1026),#720,.F.);
#5022=ADVANCED_FACE('',(#1027),#721,.F.);
#5023=ADVANCED_FACE('',(#1028),#722,.F.);
#5024=ADVANCED_FACE('',(#1029),#723,.F.);
#5025=ADVANCED_FACE('',(#1030,#543),#724,.T.);
#5026=ADVANCED_FACE('',(#1031),#33,.T.);
#5027=ADVANCED_FACE('',(#1032),#4728,.T.);
#5028=ADVANCED_FACE('',(#1033),#725,.T.);
#5029=ADVANCED_FACE('',(#1034),#34,.T.);
#5030=ADVANCED_FACE('',(#1035),#4729,.T.);
#5031=ADVANCED_FACE('',(#1036),#35,.T.);
#5032=ADVANCED_FACE('',(#1037,#544),#726,.T.);
#5033=ADVANCED_FACE('',(#1038),#36,.T.);
#5034=ADVANCED_FACE('',(#1039),#4730,.T.);
#5035=ADVANCED_FACE('',(#1040),#37,.T.);
#5036=ADVANCED_FACE('',(#1041),#727,.T.);
#5037=ADVANCED_FACE('',(#1042),#728,.F.);
#5038=ADVANCED_FACE('',(#1043),#729,.F.);
#5039=ADVANCED_FACE('',(#1044),#730,.F.);
#5040=ADVANCED_FACE('',(#1045),#731,.F.);
#5041=ADVANCED_FACE('',(#1046),#732,.F.);
#5042=ADVANCED_FACE('',(#1047),#733,.F.);
#5043=ADVANCED_FACE('',(#1048),#734,.F.);
#5044=ADVANCED_FACE('',(#1049),#735,.F.);
#5045=CLOSED_SHELL('',(#4731,#4732,#4733,#4734,#4735,#4736,#4737,#4738,
#4739,#4740,#4741,#4742,#4743,#4744,#4745));
#5046=CLOSED_SHELL('',(#4746,#4747,#4748,#4749,#4750,#4751));
#5047=CLOSED_SHELL('',(#4752,#4753,#4754,#4755,#4756,#4757));
#5048=CLOSED_SHELL('',(#4758,#4759,#4760,#4761,#4762,#4763,#4764,#4765,
#4766,#4767,#4768,#4769,#4770,#4771,#4772,#4773,#4774,#4775,#4776,#4777,
#4778,#4779,#4780,#4781,#4782));
#5049=CLOSED_SHELL('',(#4783,#4784,#4785,#4786,#4787,#4788,#4789,#4790,
#4791,#4792,#4793,#4794,#4795,#4796,#4797,#4798,#4799,#4800));
#5050=CLOSED_SHELL('',(#4801,#4802,#4803,#4804));
#5051=CLOSED_SHELL('',(#4805,#4806,#4807));
#5052=CLOSED_SHELL('',(#4808,#4809,#4810,#4811,#4812,#4813,#4814,#4815,
#4816,#4817,#4818));
#5053=CLOSED_SHELL('',(#4819,#4820,#4821,#4822,#4823,#4824,#4825,#4826,
#4827,#4828,#4829,#4830,#4831,#4832,#4833,#4834,#4835,#4836));
#5054=CLOSED_SHELL('',(#4837,#4838,#4839,#4840));
#5055=CLOSED_SHELL('',(#4841,#4842,#4843,#4844,#4845,#4846,#4847,#4848,
#4849,#4850,#4851,#4852,#4853,#4854,#4855,#4856,#4857,#4858,#4859,#4860,
#4861,#4862,#4863,#4864));
#5056=CLOSED_SHELL('',(#4865,#4866,#4867,#4868));
#5057=CLOSED_SHELL('',(#4869,#4870,#4871,#4872));
#5058=CLOSED_SHELL('',(#4873,#4874,#4875,#4876));
#5059=CLOSED_SHELL('',(#4877,#4878,#4879));
#5060=CLOSED_SHELL('',(#4880,#4881,#4882));
#5061=CLOSED_SHELL('',(#4883,#4884,#4885));
#5062=CLOSED_SHELL('',(#4886,#4887,#4888));
#5063=CLOSED_SHELL('',(#4889,#4890,#4891,#4892,#4893,#4894,#4895,#4896,
#4897,#4898,#4899,#4900,#4901,#4902,#4903,#4904,#4905));
#5064=CLOSED_SHELL('',(#4906,#4907,#4908,#4909,#4910,#4911,#4912,#4913));
#5065=CLOSED_SHELL('',(#4914,#4915,#4916,#4917,#4918,#4919,#4920,#4921,
#4922));
#5066=CLOSED_SHELL('',(#4923,#4924,#4925,#4926,#4927,#4928,#4929,#4930));
#5067=CLOSED_SHELL('',(#4931,#4932,#4933,#4934,#4935,#4936,#4937,#4938,
#4939,#4940,#4941,#4942,#4943,#4944,#4945,#4946,#4947));
#5068=CLOSED_SHELL('',(#4948,#4949,#4950,#4951,#4952,#4953));
#5069=CLOSED_SHELL('',(#4954,#4955,#4956,#4957,#4958));
#5070=CLOSED_SHELL('',(#4959,#4960,#4961,#4962,#4963,#4964,#4965,#4966,
#4967,#4968,#4969));
#5071=CLOSED_SHELL('',(#4970,#4971,#4972,#4973,#4974,#4975,#4976,#4977,
#4978,#4979,#4980,#4981,#4982,#4983,#4984,#4985,#4986,#4987,#4988,#4989,
#4990,#4991,#4992,#4993));
#5072=CLOSED_SHELL('',(#4994,#4995,#4996,#4997,#4998,#4999,#5000));
#5073=CLOSED_SHELL('',(#5001,#5002,#5003,#5004,#5005,#5006,#5007,#5008));
#5074=CLOSED_SHELL('',(#5009,#5010,#5011,#5012));
#5075=CLOSED_SHELL('',(#5013,#5014,#5015,#5016));
#5076=CLOSED_SHELL('',(#5017,#5018,#5019,#5020,#5021,#5022,#5023,#5024,
#5025,#5026,#5027));
#5077=CLOSED_SHELL('',(#5028,#5029,#5030,#5031,#5032,#5033,#5034,#5035,
#5036));
#5078=CLOSED_SHELL('',(#5037,#5038,#5039,#5040,#5041,#5042,#5043,#5044));
#5079=DERIVED_UNIT_ELEMENT(#5143,1.);
#5080=DERIVED_UNIT_ELEMENT(#10267,-3.);
#5081=DERIVED_UNIT_ELEMENT(#5143,1.);
#5082=DERIVED_UNIT_ELEMENT(#10267,-3.);
#5083=DERIVED_UNIT_ELEMENT(#5143,1.);
#5084=DERIVED_UNIT_ELEMENT(#10267,-3.);
#5085=DERIVED_UNIT_ELEMENT(#5143,1.);
#5086=DERIVED_UNIT_ELEMENT(#10267,-3.);
#5087=DERIVED_UNIT_ELEMENT(#5143,1.);
#5088=DERIVED_UNIT_ELEMENT(#10267,-3.);
#5089=DERIVED_UNIT_ELEMENT(#5143,1.);
#5090=DERIVED_UNIT_ELEMENT(#10267,-3.);
#5091=DERIVED_UNIT_ELEMENT(#5143,1.);
#5092=DERIVED_UNIT_ELEMENT(#10267,-3.);
#5093=DERIVED_UNIT_ELEMENT(#5143,1.);
#5094=DERIVED_UNIT_ELEMENT(#10267,-3.);
#5095=DERIVED_UNIT_ELEMENT(#5143,1.);
#5096=DERIVED_UNIT_ELEMENT(#10267,-3.);
#5097=DERIVED_UNIT_ELEMENT(#5143,1.);
#5098=DERIVED_UNIT_ELEMENT(#10267,-3.);
#5099=DERIVED_UNIT_ELEMENT(#5143,1.);
#5100=DERIVED_UNIT_ELEMENT(#10267,-3.);
#5101=DERIVED_UNIT_ELEMENT(#5143,1.);
#5102=DERIVED_UNIT_ELEMENT(#10267,-3.);
#5103=DERIVED_UNIT_ELEMENT(#5143,1.);
#5104=DERIVED_UNIT_ELEMENT(#10267,-3.);
#5105=DERIVED_UNIT_ELEMENT(#5143,1.);
#5106=DERIVED_UNIT_ELEMENT(#10267,-3.);
#5107=DERIVED_UNIT_ELEMENT(#5143,1.);
#5108=DERIVED_UNIT_ELEMENT(#10267,-3.);
#5109=DERIVED_UNIT_ELEMENT(#5143,1.);
#5110=DERIVED_UNIT_ELEMENT(#10267,-3.);
#5111=DERIVED_UNIT_ELEMENT(#5143,1.);
#5112=DERIVED_UNIT_ELEMENT(#10267,-3.);
#5113=DERIVED_UNIT_ELEMENT(#5143,1.);
#5114=DERIVED_UNIT_ELEMENT(#10267,-3.);
#5115=DERIVED_UNIT_ELEMENT(#5143,1.);
#5116=DERIVED_UNIT_ELEMENT(#10267,-3.);
#5117=DERIVED_UNIT_ELEMENT(#5143,1.);
#5118=DERIVED_UNIT_ELEMENT(#10267,-3.);
#5119=DERIVED_UNIT_ELEMENT(#5143,1.);
#5120=DERIVED_UNIT_ELEMENT(#10267,-3.);
#5121=DERIVED_UNIT_ELEMENT(#5143,1.);
#5122=DERIVED_UNIT_ELEMENT(#10267,-3.);
#5123=DERIVED_UNIT_ELEMENT(#5143,1.);
#5124=DERIVED_UNIT_ELEMENT(#10267,-3.);
#5125=DERIVED_UNIT_ELEMENT(#5143,1.);
#5126=DERIVED_UNIT_ELEMENT(#10267,-3.);
#5127=DERIVED_UNIT_ELEMENT(#5143,1.);
#5128=DERIVED_UNIT_ELEMENT(#10267,-3.);
#5129=DERIVED_UNIT_ELEMENT(#5143,1.);
#5130=DERIVED_UNIT_ELEMENT(#10267,-3.);
#5131=DERIVED_UNIT_ELEMENT(#5143,1.);
#5132=DERIVED_UNIT_ELEMENT(#10267,-3.);
#5133=DERIVED_UNIT_ELEMENT(#5143,1.);
#5134=DERIVED_UNIT_ELEMENT(#10267,-3.);
#5135=DERIVED_UNIT_ELEMENT(#5143,1.);
#5136=DERIVED_UNIT_ELEMENT(#10267,-3.);
#5137=DERIVED_UNIT_ELEMENT(#5143,1.);
#5138=DERIVED_UNIT_ELEMENT(#10267,-3.);
#5139=DERIVED_UNIT_ELEMENT(#5143,1.);
#5140=DERIVED_UNIT_ELEMENT(#10267,-3.);
#5141=DERIVED_UNIT_ELEMENT(#5143,1.);
#5142=DERIVED_UNIT_ELEMENT(#10267,-3.);
#5143=(
MASS_UNIT()
NAMED_UNIT(*)
SI_UNIT(.KILO.,.GRAM.)
);
#5144=DERIVED_UNIT((#5079,#5080));
#5145=DERIVED_UNIT((#5081,#5082));
#5146=DERIVED_UNIT((#5083,#5084));
#5147=DERIVED_UNIT((#5085,#5086));
#5148=DERIVED_UNIT((#5087,#5088));
#5149=DERIVED_UNIT((#5089,#5090));
#5150=DERIVED_UNIT((#5091,#5092));
#5151=DERIVED_UNIT((#5093,#5094));
#5152=DERIVED_UNIT((#5095,#5096));
#5153=DERIVED_UNIT((#5097,#5098));
#5154=DERIVED_UNIT((#5099,#5100));
#5155=DERIVED_UNIT((#5101,#5102));
#5156=DERIVED_UNIT((#5103,#5104));
#5157=DERIVED_UNIT((#5105,#5106));
#5158=DERIVED_UNIT((#5107,#5108));
#5159=DERIVED_UNIT((#5109,#5110));
#5160=DERIVED_UNIT((#5111,#5112));
#5161=DERIVED_UNIT((#5113,#5114));
#5162=DERIVED_UNIT((#5115,#5116));
#5163=DERIVED_UNIT((#5117,#5118));
#5164=DERIVED_UNIT((#5119,#5120));
#5165=DERIVED_UNIT((#5121,#5122));
#5166=DERIVED_UNIT((#5123,#5124));
#5167=DERIVED_UNIT((#5125,#5126));
#5168=DERIVED_UNIT((#5127,#5128));
#5169=DERIVED_UNIT((#5129,#5130));
#5170=DERIVED_UNIT((#5131,#5132));
#5171=DERIVED_UNIT((#5133,#5134));
#5172=DERIVED_UNIT((#5135,#5136));
#5173=DERIVED_UNIT((#5137,#5138));
#5174=DERIVED_UNIT((#5139,#5140));
#5175=DERIVED_UNIT((#5141,#5142));
#5176=MEASURE_REPRESENTATION_ITEM('density measure',
POSITIVE_RATIO_MEASURE(7850.),#5144);
#5177=MEASURE_REPRESENTATION_ITEM('density measure',
POSITIVE_RATIO_MEASURE(7850.),#5145);
#5178=MEASURE_REPRESENTATION_ITEM('density measure',
POSITIVE_RATIO_MEASURE(7850.),#5146);
#5179=MEASURE_REPRESENTATION_ITEM('density measure',
POSITIVE_RATIO_MEASURE(7850.),#5147);
#5180=MEASURE_REPRESENTATION_ITEM('density measure',
POSITIVE_RATIO_MEASURE(7850.),#5148);
#5181=MEASURE_REPRESENTATION_ITEM('density measure',
POSITIVE_RATIO_MEASURE(7850.),#5149);
#5182=MEASURE_REPRESENTATION_ITEM('density measure',
POSITIVE_RATIO_MEASURE(7850.),#5150);
#5183=MEASURE_REPRESENTATION_ITEM('density measure',
POSITIVE_RATIO_MEASURE(7850.),#5151);
#5184=MEASURE_REPRESENTATION_ITEM('density measure',
POSITIVE_RATIO_MEASURE(7850.),#5152);
#5185=MEASURE_REPRESENTATION_ITEM('density measure',
POSITIVE_RATIO_MEASURE(7850.),#5153);
#5186=MEASURE_REPRESENTATION_ITEM('density measure',
POSITIVE_RATIO_MEASURE(7850.),#5154);
#5187=MEASURE_REPRESENTATION_ITEM('density measure',
POSITIVE_RATIO_MEASURE(7850.),#5155);
#5188=MEASURE_REPRESENTATION_ITEM('density measure',
POSITIVE_RATIO_MEASURE(7850.),#5156);
#5189=MEASURE_REPRESENTATION_ITEM('density measure',
POSITIVE_RATIO_MEASURE(7850.),#5157);
#5190=MEASURE_REPRESENTATION_ITEM('density measure',
POSITIVE_RATIO_MEASURE(7850.),#5158);
#5191=MEASURE_REPRESENTATION_ITEM('density measure',
POSITIVE_RATIO_MEASURE(7850.),#5159);
#5192=MEASURE_REPRESENTATION_ITEM('density measure',
POSITIVE_RATIO_MEASURE(7850.),#5160);
#5193=MEASURE_REPRESENTATION_ITEM('density measure',
POSITIVE_RATIO_MEASURE(7850.),#5161);
#5194=MEASURE_REPRESENTATION_ITEM('density measure',
POSITIVE_RATIO_MEASURE(7850.),#5162);
#5195=MEASURE_REPRESENTATION_ITEM('density measure',
POSITIVE_RATIO_MEASURE(7850.),#5163);
#5196=MEASURE_REPRESENTATION_ITEM('density measure',
POSITIVE_RATIO_MEASURE(7850.),#5164);
#5197=MEASURE_REPRESENTATION_ITEM('density measure',
POSITIVE_RATIO_MEASURE(7850.),#5165);
#5198=MEASURE_REPRESENTATION_ITEM('density measure',
POSITIVE_RATIO_MEASURE(7850.),#5166);
#5199=MEASURE_REPRESENTATION_ITEM('density measure',
POSITIVE_RATIO_MEASURE(7850.),#5167);
#5200=MEASURE_REPRESENTATION_ITEM('density measure',
POSITIVE_RATIO_MEASURE(7850.),#5168);
#5201=MEASURE_REPRESENTATION_ITEM('density measure',
POSITIVE_RATIO_MEASURE(7850.),#5169);
#5202=MEASURE_REPRESENTATION_ITEM('density measure',
POSITIVE_RATIO_MEASURE(7850.),#5170);
#5203=MEASURE_REPRESENTATION_ITEM('density measure',
POSITIVE_RATIO_MEASURE(7850.),#5171);
#5204=MEASURE_REPRESENTATION_ITEM('density measure',
POSITIVE_RATIO_MEASURE(7850.),#5172);
#5205=MEASURE_REPRESENTATION_ITEM('density measure',
POSITIVE_RATIO_MEASURE(7850.),#5173);
#5206=MEASURE_REPRESENTATION_ITEM('density measure',
POSITIVE_RATIO_MEASURE(7850.),#5174);
#5207=MEASURE_REPRESENTATION_ITEM('density measure',
POSITIVE_RATIO_MEASURE(7850.),#5175);
#5208=PROPERTY_DEFINITION_REPRESENTATION(#5368,#5272);
#5209=PROPERTY_DEFINITION_REPRESENTATION(#5369,#5273);
#5210=PROPERTY_DEFINITION_REPRESENTATION(#5370,#5274);
#5211=PROPERTY_DEFINITION_REPRESENTATION(#5371,#5275);
#5212=PROPERTY_DEFINITION_REPRESENTATION(#5372,#5276);
#5213=PROPERTY_DEFINITION_REPRESENTATION(#5373,#5277);
#5214=PROPERTY_DEFINITION_REPRESENTATION(#5374,#5278);
#5215=PROPERTY_DEFINITION_REPRESENTATION(#5375,#5279);
#5216=PROPERTY_DEFINITION_REPRESENTATION(#5376,#5280);
#5217=PROPERTY_DEFINITION_REPRESENTATION(#5377,#5281);
#5218=PROPERTY_DEFINITION_REPRESENTATION(#5378,#5282);
#5219=PROPERTY_DEFINITION_REPRESENTATION(#5379,#5283);
#5220=PROPERTY_DEFINITION_REPRESENTATION(#5380,#5284);
#5221=PROPERTY_DEFINITION_REPRESENTATION(#5381,#5285);
#5222=PROPERTY_DEFINITION_REPRESENTATION(#5382,#5286);
#5223=PROPERTY_DEFINITION_REPRESENTATION(#5383,#5287);
#5224=PROPERTY_DEFINITION_REPRESENTATION(#5384,#5288);
#5225=PROPERTY_DEFINITION_REPRESENTATION(#5385,#5289);
#5226=PROPERTY_DEFINITION_REPRESENTATION(#5386,#5290);
#5227=PROPERTY_DEFINITION_REPRESENTATION(#5387,#5291);
#5228=PROPERTY_DEFINITION_REPRESENTATION(#5388,#5292);
#5229=PROPERTY_DEFINITION_REPRESENTATION(#5389,#5293);
#5230=PROPERTY_DEFINITION_REPRESENTATION(#5390,#5294);
#5231=PROPERTY_DEFINITION_REPRESENTATION(#5391,#5295);
#5232=PROPERTY_DEFINITION_REPRESENTATION(#5392,#5296);
#5233=PROPERTY_DEFINITION_REPRESENTATION(#5393,#5297);
#5234=PROPERTY_DEFINITION_REPRESENTATION(#5394,#5298);
#5235=PROPERTY_DEFINITION_REPRESENTATION(#5395,#5299);
#5236=PROPERTY_DEFINITION_REPRESENTATION(#5396,#5300);
#5237=PROPERTY_DEFINITION_REPRESENTATION(#5397,#5301);
#5238=PROPERTY_DEFINITION_REPRESENTATION(#5398,#5302);
#5239=PROPERTY_DEFINITION_REPRESENTATION(#5399,#5303);
#5240=PROPERTY_DEFINITION_REPRESENTATION(#5400,#5304);
#5241=PROPERTY_DEFINITION_REPRESENTATION(#5401,#5305);
#5242=PROPERTY_DEFINITION_REPRESENTATION(#5402,#5306);
#5243=PROPERTY_DEFINITION_REPRESENTATION(#5403,#5307);
#5244=PROPERTY_DEFINITION_REPRESENTATION(#5404,#5308);
#5245=PROPERTY_DEFINITION_REPRESENTATION(#5405,#5309);
#5246=PROPERTY_DEFINITION_REPRESENTATION(#5406,#5310);
#5247=PROPERTY_DEFINITION_REPRESENTATION(#5407,#5311);
#5248=PROPERTY_DEFINITION_REPRESENTATION(#5408,#5312);
#5249=PROPERTY_DEFINITION_REPRESENTATION(#5409,#5313);
#5250=PROPERTY_DEFINITION_REPRESENTATION(#5410,#5314);
#5251=PROPERTY_DEFINITION_REPRESENTATION(#5411,#5315);
#5252=PROPERTY_DEFINITION_REPRESENTATION(#5412,#5316);
#5253=PROPERTY_DEFINITION_REPRESENTATION(#5413,#5317);
#5254=PROPERTY_DEFINITION_REPRESENTATION(#5414,#5318);
#5255=PROPERTY_DEFINITION_REPRESENTATION(#5415,#5319);
#5256=PROPERTY_DEFINITION_REPRESENTATION(#5416,#5320);
#5257=PROPERTY_DEFINITION_REPRESENTATION(#5417,#5321);
#5258=PROPERTY_DEFINITION_REPRESENTATION(#5418,#5322);
#5259=PROPERTY_DEFINITION_REPRESENTATION(#5419,#5323);
#5260=PROPERTY_DEFINITION_REPRESENTATION(#5420,#5324);
#5261=PROPERTY_DEFINITION_REPRESENTATION(#5421,#5325);
#5262=PROPERTY_DEFINITION_REPRESENTATION(#5422,#5326);
#5263=PROPERTY_DEFINITION_REPRESENTATION(#5423,#5327);
#5264=PROPERTY_DEFINITION_REPRESENTATION(#5424,#5328);
#5265=PROPERTY_DEFINITION_REPRESENTATION(#5425,#5329);
#5266=PROPERTY_DEFINITION_REPRESENTATION(#5426,#5330);
#5267=PROPERTY_DEFINITION_REPRESENTATION(#5427,#5331);
#5268=PROPERTY_DEFINITION_REPRESENTATION(#5428,#5332);
#5269=PROPERTY_DEFINITION_REPRESENTATION(#5429,#5333);
#5270=PROPERTY_DEFINITION_REPRESENTATION(#5430,#5334);
#5271=PROPERTY_DEFINITION_REPRESENTATION(#5431,#5335);
#5272=REPRESENTATION('material name',(#5336),#10230);
#5273=REPRESENTATION('density',(#5176),#10230);
#5274=REPRESENTATION('material name',(#5337),#10231);
#5275=REPRESENTATION('density',(#5177),#10231);
#5276=REPRESENTATION('material name',(#5338),#10232);
#5277=REPRESENTATION('density',(#5178),#10232);
#5278=REPRESENTATION('material name',(#5339),#10233);
#5279=REPRESENTATION('density',(#5179),#10233);
#5280=REPRESENTATION('material name',(#5340),#10234);
#5281=REPRESENTATION('density',(#5180),#10234);
#5282=REPRESENTATION('material name',(#5341),#10235);
#5283=REPRESENTATION('density',(#5181),#10235);
#5284=REPRESENTATION('material name',(#5342),#10236);
#5285=REPRESENTATION('density',(#5182),#10236);
#5286=REPRESENTATION('material name',(#5343),#10237);
#5287=REPRESENTATION('density',(#5183),#10237);
#5288=REPRESENTATION('material name',(#5344),#10238);
#5289=REPRESENTATION('density',(#5184),#10238);
#5290=REPRESENTATION('material name',(#5345),#10239);
#5291=REPRESENTATION('density',(#5185),#10239);
#5292=REPRESENTATION('material name',(#5346),#10240);
#5293=REPRESENTATION('density',(#5186),#10240);
#5294=REPRESENTATION('material name',(#5347),#10241);
#5295=REPRESENTATION('density',(#5187),#10241);
#5296=REPRESENTATION('material name',(#5348),#10242);
#5297=REPRESENTATION('density',(#5188),#10242);
#5298=REPRESENTATION('material name',(#5349),#10243);
#5299=REPRESENTATION('density',(#5189),#10243);
#5300=REPRESENTATION('material name',(#5350),#10244);
#5301=REPRESENTATION('density',(#5190),#10244);
#5302=REPRESENTATION('material name',(#5351),#10245);
#5303=REPRESENTATION('density',(#5191),#10245);
#5304=REPRESENTATION('material name',(#5352),#10246);
#5305=REPRESENTATION('density',(#5192),#10246);
#5306=REPRESENTATION('material name',(#5353),#10247);
#5307=REPRESENTATION('density',(#5193),#10247);
#5308=REPRESENTATION('material name',(#5354),#10249);
#5309=REPRESENTATION('density',(#5194),#10249);
#5310=REPRESENTATION('material name',(#5355),#10250);
#5311=REPRESENTATION('density',(#5195),#10250);
#5312=REPRESENTATION('material name',(#5356),#10251);
#5313=REPRESENTATION('density',(#5196),#10251);
#5314=REPRESENTATION('material name',(#5357),#10253);
#5315=REPRESENTATION('density',(#5197),#10253);
#5316=REPRESENTATION('material name',(#5358),#10254);
#5317=REPRESENTATION('density',(#5198),#10254);
#5318=REPRESENTATION('material name',(#5359),#10255);
#5319=REPRESENTATION('density',(#5199),#10255);
#5320=REPRESENTATION('material name',(#5360),#10256);
#5321=REPRESENTATION('density',(#5200),#10256);
#5322=REPRESENTATION('material name',(#5361),#10258);
#5323=REPRESENTATION('density',(#5201),#10258);
#5324=REPRESENTATION('material name',(#5362),#10259);
#5325=REPRESENTATION('density',(#5202),#10259);
#5326=REPRESENTATION('material name',(#5363),#10260);
#5327=REPRESENTATION('density',(#5203),#10260);
#5328=REPRESENTATION('material name',(#5364),#10261);
#5329=REPRESENTATION('density',(#5204),#10261);
#5330=REPRESENTATION('material name',(#5365),#10262);
#5331=REPRESENTATION('density',(#5205),#10262);
#5332=REPRESENTATION('material name',(#5366),#10263);
#5333=REPRESENTATION('density',(#5206),#10263);
#5334=REPRESENTATION('material name',(#5367),#10264);
#5335=REPRESENTATION('density',(#5207),#10264);
#5336=DESCRIPTIVE_REPRESENTATION_ITEM('Steel','Steel');
#5337=DESCRIPTIVE_REPRESENTATION_ITEM('Steel','Steel');
#5338=DESCRIPTIVE_REPRESENTATION_ITEM('Steel','Steel');
#5339=DESCRIPTIVE_REPRESENTATION_ITEM('Steel','Steel');
#5340=DESCRIPTIVE_REPRESENTATION_ITEM('Steel','Steel');
#5341=DESCRIPTIVE_REPRESENTATION_ITEM('Steel','Steel');
#5342=DESCRIPTIVE_REPRESENTATION_ITEM('Steel','Steel');
#5343=DESCRIPTIVE_REPRESENTATION_ITEM('Steel','Steel');
#5344=DESCRIPTIVE_REPRESENTATION_ITEM('Steel','Steel');
#5345=DESCRIPTIVE_REPRESENTATION_ITEM('Steel','Steel');
#5346=DESCRIPTIVE_REPRESENTATION_ITEM('Steel','Steel');
#5347=DESCRIPTIVE_REPRESENTATION_ITEM('Steel','Steel');
#5348=DESCRIPTIVE_REPRESENTATION_ITEM('Steel','Steel');
#5349=DESCRIPTIVE_REPRESENTATION_ITEM('Steel','Steel');
#5350=DESCRIPTIVE_REPRESENTATION_ITEM('Steel','Steel');
#5351=DESCRIPTIVE_REPRESENTATION_ITEM('Steel','Steel');
#5352=DESCRIPTIVE_REPRESENTATION_ITEM('Steel','Steel');
#5353=DESCRIPTIVE_REPRESENTATION_ITEM('Steel','Steel');
#5354=DESCRIPTIVE_REPRESENTATION_ITEM('Steel','Steel');
#5355=DESCRIPTIVE_REPRESENTATION_ITEM('Steel','Steel');
#5356=DESCRIPTIVE_REPRESENTATION_ITEM('Steel','Steel');
#5357=DESCRIPTIVE_REPRESENTATION_ITEM('Steel','Steel');
#5358=DESCRIPTIVE_REPRESENTATION_ITEM('Steel','Steel');
#5359=DESCRIPTIVE_REPRESENTATION_ITEM('Steel','Steel');
#5360=DESCRIPTIVE_REPRESENTATION_ITEM('Steel','Steel');
#5361=DESCRIPTIVE_REPRESENTATION_ITEM('Steel','Steel');
#5362=DESCRIPTIVE_REPRESENTATION_ITEM('Steel','Steel');
#5363=DESCRIPTIVE_REPRESENTATION_ITEM('Steel','Steel');
#5364=DESCRIPTIVE_REPRESENTATION_ITEM('Steel','Steel');
#5365=DESCRIPTIVE_REPRESENTATION_ITEM('Steel','Steel');
#5366=DESCRIPTIVE_REPRESENTATION_ITEM('Steel','Steel');
#5367=DESCRIPTIVE_REPRESENTATION_ITEM('Steel','Steel');
#5368=PROPERTY_DEFINITION('material property','material name',#10444);
#5369=PROPERTY_DEFINITION('material property','density of part',#10444);
#5370=PROPERTY_DEFINITION('material property','material name',#10445);
#5371=PROPERTY_DEFINITION('material property','density of part',#10445);
#5372=PROPERTY_DEFINITION('material property','material name',#10446);
#5373=PROPERTY_DEFINITION('material property','density of part',#10446);
#5374=PROPERTY_DEFINITION('material property','material name',#10447);
#5375=PROPERTY_DEFINITION('material property','density of part',#10447);
#5376=PROPERTY_DEFINITION('material property','material name',#10448);
#5377=PROPERTY_DEFINITION('material property','density of part',#10448);
#5378=PROPERTY_DEFINITION('material property','material name',#10449);
#5379=PROPERTY_DEFINITION('material property','density of part',#10449);
#5380=PROPERTY_DEFINITION('material property','material name',#10450);
#5381=PROPERTY_DEFINITION('material property','density of part',#10450);
#5382=PROPERTY_DEFINITION('material property','material name',#10451);
#5383=PROPERTY_DEFINITION('material property','density of part',#10451);
#5384=PROPERTY_DEFINITION('material property','material name',#10452);
#5385=PROPERTY_DEFINITION('material property','density of part',#10452);
#5386=PROPERTY_DEFINITION('material property','material name',#10453);
#5387=PROPERTY_DEFINITION('material property','density of part',#10453);
#5388=PROPERTY_DEFINITION('material property','material name',#10454);
#5389=PROPERTY_DEFINITION('material property','density of part',#10454);
#5390=PROPERTY_DEFINITION('material property','material name',#10455);
#5391=PROPERTY_DEFINITION('material property','density of part',#10455);
#5392=PROPERTY_DEFINITION('material property','material name',#10456);
#5393=PROPERTY_DEFINITION('material property','density of part',#10456);
#5394=PROPERTY_DEFINITION('material property','material name',#10457);
#5395=PROPERTY_DEFINITION('material property','density of part',#10457);
#5396=PROPERTY_DEFINITION('material property','material name',#10458);
#5397=PROPERTY_DEFINITION('material property','density of part',#10458);
#5398=PROPERTY_DEFINITION('material property','material name',#10459);
#5399=PROPERTY_DEFINITION('material property','density of part',#10459);
#5400=PROPERTY_DEFINITION('material property','material name',#10460);
#5401=PROPERTY_DEFINITION('material property','density of part',#10460);
#5402=PROPERTY_DEFINITION('material property','material name',#10461);
#5403=PROPERTY_DEFINITION('material property','density of part',#10461);
#5404=PROPERTY_DEFINITION('material property','material name',#10463);
#5405=PROPERTY_DEFINITION('material property','density of part',#10463);
#5406=PROPERTY_DEFINITION('material property','material name',#10464);
#5407=PROPERTY_DEFINITION('material property','density of part',#10464);
#5408=PROPERTY_DEFINITION('material property','material name',#10465);
#5409=PROPERTY_DEFINITION('material property','density of part',#10465);
#5410=PROPERTY_DEFINITION('material property','material name',#10467);
#5411=PROPERTY_DEFINITION('material property','density of part',#10467);
#5412=PROPERTY_DEFINITION('material property','material name',#10468);
#5413=PROPERTY_DEFINITION('material property','density of part',#10468);
#5414=PROPERTY_DEFINITION('material property','material name',#10469);
#5415=PROPERTY_DEFINITION('material property','density of part',#10469);
#5416=PROPERTY_DEFINITION('material property','material name',#10470);
#5417=PROPERTY_DEFINITION('material property','density of part',#10470);
#5418=PROPERTY_DEFINITION('material property','material name',#10472);
#5419=PROPERTY_DEFINITION('material property','density of part',#10472);
#5420=PROPERTY_DEFINITION('material property','material name',#10473);
#5421=PROPERTY_DEFINITION('material property','density of part',#10473);
#5422=PROPERTY_DEFINITION('material property','material name',#10474);
#5423=PROPERTY_DEFINITION('material property','density of part',#10474);
#5424=PROPERTY_DEFINITION('material property','material name',#10475);
#5425=PROPERTY_DEFINITION('material property','density of part',#10475);
#5426=PROPERTY_DEFINITION('material property','material name',#10476);
#5427=PROPERTY_DEFINITION('material property','density of part',#10476);
#5428=PROPERTY_DEFINITION('material property','material name',#10477);
#5429=PROPERTY_DEFINITION('material property','density of part',#10477);
#5430=PROPERTY_DEFINITION('material property','material name',#10478);
#5431=PROPERTY_DEFINITION('material property','density of part',#10478);
#5432=AXIS2_PLACEMENT_3D('',#7738,#6089,#6090);
#5433=AXIS2_PLACEMENT_3D('',#7739,#6091,#6092);
#5434=AXIS2_PLACEMENT_3D('',#7740,#6093,#6094);
#5435=AXIS2_PLACEMENT_3D('',#7741,#6095,#6096);
#5436=AXIS2_PLACEMENT_3D('',#7743,#6097,#6098);
#5437=AXIS2_PLACEMENT_3D('',#7746,#6100,#6101);
#5438=AXIS2_PLACEMENT_3D('',#7747,#6102,#6103);
#5439=AXIS2_PLACEMENT_3D('',#7749,#6104,#6105);
#5440=AXIS2_PLACEMENT_3D('',#7752,#6107,#6108);
#5441=AXIS2_PLACEMENT_3D('',#7753,#6109,#6110);
#5442=AXIS2_PLACEMENT_3D('',#7755,#6111,#6112);
#5443=AXIS2_PLACEMENT_3D('',#7758,#6114,#6115);
#5444=AXIS2_PLACEMENT_3D('',#7759,#6116,#6117);
#5445=AXIS2_PLACEMENT_3D('',#7761,#6118,#6119);
#5446=AXIS2_PLACEMENT_3D('',#7764,#6121,#6122);
#5447=AXIS2_PLACEMENT_3D('',#7765,#6123,#6124);
#5448=AXIS2_PLACEMENT_3D('',#7767,#6125,#6126);
#5449=AXIS2_PLACEMENT_3D('',#7770,#6128,#6129);
#5450=AXIS2_PLACEMENT_3D('',#7771,#6130,#6131);
#5451=AXIS2_PLACEMENT_3D('',#7773,#6132,#6133);
#5452=AXIS2_PLACEMENT_3D('',#7776,#6135,#6136);
#5453=AXIS2_PLACEMENT_3D('',#7777,#6137,#6138);
#5454=AXIS2_PLACEMENT_3D('',#7779,#6139,#6140);
#5455=AXIS2_PLACEMENT_3D('',#7782,#6142,#6143);
#5456=AXIS2_PLACEMENT_3D('',#7783,#6144,#6145);
#5457=AXIS2_PLACEMENT_3D('',#7785,#6146,#6147);
#5458=AXIS2_PLACEMENT_3D('',#7788,#6149,#6150);
#5459=AXIS2_PLACEMENT_3D('',#7789,#6151,#6152);
#5460=AXIS2_PLACEMENT_3D('',#7791,#6153,#6154);
#5461=AXIS2_PLACEMENT_3D('',#7794,#6156,#6157);
#5462=AXIS2_PLACEMENT_3D('',#7795,#6158,#6159);
#5463=AXIS2_PLACEMENT_3D('',#7804,#6164,#6165);
#5464=AXIS2_PLACEMENT_3D('',#7810,#6169,#6170);
#5465=AXIS2_PLACEMENT_3D('',#7816,#6174,#6175);
#5466=AXIS2_PLACEMENT_3D('',#7819,#6178,#6179);
#5467=AXIS2_PLACEMENT_3D('',#7820,#6180,#6181);
#5468=AXIS2_PLACEMENT_3D('',#7821,#6182,#6183);
#5469=AXIS2_PLACEMENT_3D('',#7822,#6184,#6185);
#5470=AXIS2_PLACEMENT_3D('',#7831,#6190,#6191);
#5471=AXIS2_PLACEMENT_3D('',#7837,#6195,#6196);
#5472=AXIS2_PLACEMENT_3D('',#7843,#6200,#6201);
#5473=AXIS2_PLACEMENT_3D('',#7846,#6204,#6205);
#5474=AXIS2_PLACEMENT_3D('',#7847,#6206,#6207);
#5475=AXIS2_PLACEMENT_3D('',#7848,#6208,#6209);
#5476=AXIS2_PLACEMENT_3D('',#7849,#6210,#6211);
#5477=AXIS2_PLACEMENT_3D('',#7858,#6216,#6217);
#5478=AXIS2_PLACEMENT_3D('',#7864,#6221,#6222);
#5479=AXIS2_PLACEMENT_3D('',#7870,#6226,#6227);
#5480=AXIS2_PLACEMENT_3D('',#7873,#6230,#6231);
#5481=AXIS2_PLACEMENT_3D('',#7874,#6232,#6233);
#5482=AXIS2_PLACEMENT_3D('',#7875,#6234,#6235);
#5483=AXIS2_PLACEMENT_3D('',#7876,#6236,#6237);
#5484=AXIS2_PLACEMENT_3D('',#7878,#6238,#6239);
#5485=AXIS2_PLACEMENT_3D('',#7881,#6241,#6242);
#5486=AXIS2_PLACEMENT_3D('',#7882,#6243,#6244);
#5487=AXIS2_PLACEMENT_3D('',#7883,#6245,#6246);
#5488=AXIS2_PLACEMENT_3D('',#7885,#6247,#6248);
#5489=AXIS2_PLACEMENT_3D('',#7888,#6250,#6251);
#5490=AXIS2_PLACEMENT_3D('',#7889,#6252,#6253);
#5491=AXIS2_PLACEMENT_3D('',#7890,#6254,#6255);
#5492=AXIS2_PLACEMENT_3D('',#7892,#6256,#6257);
#5493=AXIS2_PLACEMENT_3D('',#7895,#6259,#6260);
#5494=AXIS2_PLACEMENT_3D('',#7896,#6261,#6262);
#5495=AXIS2_PLACEMENT_3D('',#7897,#6263,#6264);
#5496=AXIS2_PLACEMENT_3D('',#7899,#6265,#6266);
#5497=AXIS2_PLACEMENT_3D('',#7902,#6268,#6269);
#5498=AXIS2_PLACEMENT_3D('',#7903,#6270,#6271);
#5499=AXIS2_PLACEMENT_3D('',#7904,#6272,#6273);
#5500=AXIS2_PLACEMENT_3D('',#7906,#6274,#6275);
#5501=AXIS2_PLACEMENT_3D('',#7909,#6277,#6278);
#5502=AXIS2_PLACEMENT_3D('',#7910,#6279,#6280);
#5503=AXIS2_PLACEMENT_3D('',#7911,#6281,#6282);
#5504=AXIS2_PLACEMENT_3D('',#7913,#6283,#6284);
#5505=AXIS2_PLACEMENT_3D('',#7916,#6286,#6287);
#5506=AXIS2_PLACEMENT_3D('',#7917,#6288,#6289);
#5507=AXIS2_PLACEMENT_3D('',#7918,#6290,#6291);
#5508=AXIS2_PLACEMENT_3D('',#7920,#6292,#6293);
#5509=AXIS2_PLACEMENT_3D('',#7923,#6295,#6296);
#5510=AXIS2_PLACEMENT_3D('',#7924,#6297,#6298);
#5511=AXIS2_PLACEMENT_3D('',#7925,#6299,#6300);
#5512=AXIS2_PLACEMENT_3D('',#7927,#6301,#6302);
#5513=AXIS2_PLACEMENT_3D('',#7930,#6304,#6305);
#5514=AXIS2_PLACEMENT_3D('',#7931,#6306,#6307);
#5515=AXIS2_PLACEMENT_3D('',#7932,#6308,#6309);
#5516=AXIS2_PLACEMENT_3D('',#7934,#6310,#6311);
#5517=AXIS2_PLACEMENT_3D('',#7937,#6313,#6314);
#5518=AXIS2_PLACEMENT_3D('',#7938,#6315,#6316);
#5519=AXIS2_PLACEMENT_3D('',#7940,#6317,#6318);
#5520=AXIS2_PLACEMENT_3D('',#7941,#6319,#6320);
#5521=AXIS2_PLACEMENT_3D('',#7943,#6321,#6322);
#5522=AXIS2_PLACEMENT_3D('',#7945,#6324,#6325);
#5523=AXIS2_PLACEMENT_3D('',#7954,#6330,#6331);
#5524=AXIS2_PLACEMENT_3D('',#7960,#6335,#6336);
#5525=AXIS2_PLACEMENT_3D('',#7966,#6340,#6341);
#5526=AXIS2_PLACEMENT_3D('',#7969,#6344,#6345);
#5527=AXIS2_PLACEMENT_3D('',#7970,#6346,#6347);
#5528=AXIS2_PLACEMENT_3D('',#7971,#6348,#6349);
#5529=AXIS2_PLACEMENT_3D('',#7972,#6350,#6351);
#5530=AXIS2_PLACEMENT_3D('',#7974,#6352,#6353);
#5531=AXIS2_PLACEMENT_3D('',#7977,#6355,#6356);
#5532=AXIS2_PLACEMENT_3D('',#7978,#6357,#6358);
#5533=AXIS2_PLACEMENT_3D('',#7980,#6359,#6360);
#5534=AXIS2_PLACEMENT_3D('',#7981,#6361,#6362);
#5535=AXIS2_PLACEMENT_3D('',#7983,#6363,#6364);
#5536=AXIS2_PLACEMENT_3D('',#7986,#6366,#6367);
#5537=AXIS2_PLACEMENT_3D('',#7987,#6368,#6369);
#5538=AXIS2_PLACEMENT_3D('',#7989,#6370,#6371);
#5539=AXIS2_PLACEMENT_3D('',#7990,#6372,#6373);
#5540=AXIS2_PLACEMENT_3D('',#7992,#6374,#6375);
#5541=AXIS2_PLACEMENT_3D('',#7995,#6377,#6378);
#5542=AXIS2_PLACEMENT_3D('',#7996,#6379,#6380);
#5543=AXIS2_PLACEMENT_3D('',#7998,#6381,#6382);
#5544=AXIS2_PLACEMENT_3D('',#7999,#6383,#6384);
#5545=AXIS2_PLACEMENT_3D('',#8001,#6385,#6386);
#5546=AXIS2_PLACEMENT_3D('',#8004,#6388,#6389);
#5547=AXIS2_PLACEMENT_3D('',#8005,#6390,#6391);
#5548=AXIS2_PLACEMENT_3D('',#8007,#6392,#6393);
#5549=AXIS2_PLACEMENT_3D('',#8008,#6394,#6395);
#5550=AXIS2_PLACEMENT_3D('',#8010,#6396,#6397);
#5551=AXIS2_PLACEMENT_3D('',#8012,#6399,#6400);
#5552=AXIS2_PLACEMENT_3D('',#8014,#6401,#6402);
#5553=AXIS2_PLACEMENT_3D('',#8016,#6404,#6405);
#5554=AXIS2_PLACEMENT_3D('',#8018,#6406,#6407);
#5555=AXIS2_PLACEMENT_3D('',#8020,#6409,#6410);
#5556=AXIS2_PLACEMENT_3D('',#8022,#6411,#6412);
#5557=AXIS2_PLACEMENT_3D('',#8024,#6414,#6415);
#5558=AXIS2_PLACEMENT_3D('',#8026,#6416,#6417);
#5559=AXIS2_PLACEMENT_3D('',#8029,#6419,#6420);
#5560=AXIS2_PLACEMENT_3D('',#8030,#6421,#6422);
#5561=AXIS2_PLACEMENT_3D('',#8032,#6423,#6424);
#5562=AXIS2_PLACEMENT_3D('',#8033,#6425,#6426);
#5563=AXIS2_PLACEMENT_3D('',#8035,#6427,#6428);
#5564=AXIS2_PLACEMENT_3D('',#8037,#6430,#6431);
#5565=AXIS2_PLACEMENT_3D('',#8039,#6432,#6433);
#5566=AXIS2_PLACEMENT_3D('',#8042,#6435,#6436);
#5567=AXIS2_PLACEMENT_3D('',#8043,#6437,#6438);
#5568=AXIS2_PLACEMENT_3D('',#8044,#6439,#6440);
#5569=AXIS2_PLACEMENT_3D('',#8045,#6441,#6442);
#5570=AXIS2_PLACEMENT_3D('',#8046,#6443,#6444);
#5571=AXIS2_PLACEMENT_3D('',#8048,#6445,#6446);
#5572=AXIS2_PLACEMENT_3D('',#8051,#6448,#6449);
#5573=AXIS2_PLACEMENT_3D('',#8052,#6450,#6451);
#5574=AXIS2_PLACEMENT_3D('',#8054,#6452,#6453);
#5575=AXIS2_PLACEMENT_3D('',#8057,#6455,#6456);
#5576=AXIS2_PLACEMENT_3D('',#8058,#6457,#6458);
#5577=AXIS2_PLACEMENT_3D('',#8059,#6459,#6460);
#5578=AXIS2_PLACEMENT_3D('',#8060,#6461,#6462);
#5579=AXIS2_PLACEMENT_3D('',#8822,#6463,#6464);
#5580=AXIS2_PLACEMENT_3D('',#8900,#6465,#6466);
#5581=AXIS2_PLACEMENT_3D('',#8901,#6467,#6468);
#5582=AXIS2_PLACEMENT_3D('',#8902,#6469,#6470);
#5583=AXIS2_PLACEMENT_3D('',#8903,#6471,#6472);
#5584=AXIS2_PLACEMENT_3D('',#8904,#6473,#6474);
#5585=AXIS2_PLACEMENT_3D('',#8906,#6475,#6476);
#5586=AXIS2_PLACEMENT_3D('',#8909,#6478,#6479);
#5587=AXIS2_PLACEMENT_3D('',#8910,#6480,#6481);
#5588=AXIS2_PLACEMENT_3D('',#8911,#6482,#6483);
#5589=AXIS2_PLACEMENT_3D('',#8924,#6490,#6491);
#5590=AXIS2_PLACEMENT_3D('',#8930,#6495,#6496);
#5591=AXIS2_PLACEMENT_3D('',#8934,#6499,#6500);
#5592=AXIS2_PLACEMENT_3D('',#8942,#6505,#6506);
#5593=AXIS2_PLACEMENT_3D('',#8947,#6510,#6511);
#5594=AXIS2_PLACEMENT_3D('',#8951,#6514,#6515);
#5595=AXIS2_PLACEMENT_3D('',#8953,#6517,#6518);
#5596=AXIS2_PLACEMENT_3D('',#8954,#6519,#6520);
#5597=AXIS2_PLACEMENT_3D('',#8955,#6521,#6522);
#5598=AXIS2_PLACEMENT_3D('',#8956,#6523,#6524);
#5599=AXIS2_PLACEMENT_3D('',#8961,#6526,#6527);
#5600=AXIS2_PLACEMENT_3D('',#8990,#6529,#6530);
#5601=AXIS2_PLACEMENT_3D('',#8994,#6532,#6533);
#5602=AXIS2_PLACEMENT_3D('',#8995,#6534,#6535);
#5603=AXIS2_PLACEMENT_3D('',#9019,#6538,#6539);
#5604=AXIS2_PLACEMENT_3D('',#9021,#6541,#6542);
#5605=AXIS2_PLACEMENT_3D('',#9023,#6543,#6544);
#5606=AXIS2_PLACEMENT_3D('',#9024,#6545,#6546);
#5607=AXIS2_PLACEMENT_3D('',#9025,#6547,#6548);
#5608=AXIS2_PLACEMENT_3D('',#9027,#6549,#6550);
#5609=AXIS2_PLACEMENT_3D('',#9030,#6552,#6553);
#5610=AXIS2_PLACEMENT_3D('',#9031,#6554,#6555);
#5611=AXIS2_PLACEMENT_3D('',#9032,#6556,#6557);
#5612=AXIS2_PLACEMENT_3D('',#9044,#6559,#6560);
#5613=AXIS2_PLACEMENT_3D('',#9045,#6561,#6562);
#5614=AXIS2_PLACEMENT_3D('',#9046,#6563,#6564);
#5615=AXIS2_PLACEMENT_3D('',#9048,#6565,#6566);
#5616=AXIS2_PLACEMENT_3D('',#9049,#6567,#6568);
#5617=AXIS2_PLACEMENT_3D('',#9052,#6570,#6571);
#5618=AXIS2_PLACEMENT_3D('',#9053,#6572,#6573);
#5619=AXIS2_PLACEMENT_3D('',#9055,#6574,#6575);
#5620=AXIS2_PLACEMENT_3D('',#9058,#6577,#6578);
#5621=AXIS2_PLACEMENT_3D('',#9059,#6579,#6580);
#5622=AXIS2_PLACEMENT_3D('',#9061,#6581,#6582);
#5623=AXIS2_PLACEMENT_3D('',#9062,#6583,#6584);
#5624=AXIS2_PLACEMENT_3D('',#9064,#6586,#6587);
#5625=AXIS2_PLACEMENT_3D('',#9066,#6588,#6589);
#5626=AXIS2_PLACEMENT_3D('',#9069,#6591,#6592);
#5627=AXIS2_PLACEMENT_3D('',#9070,#6593,#6594);
#5628=AXIS2_PLACEMENT_3D('',#9072,#6595,#6596);
#5629=AXIS2_PLACEMENT_3D('',#9075,#6598,#6599);
#5630=AXIS2_PLACEMENT_3D('',#9076,#6600,#6601);
#5631=AXIS2_PLACEMENT_3D('',#9078,#6602,#6603);
#5632=AXIS2_PLACEMENT_3D('',#9081,#6605,#6606);
#5633=AXIS2_PLACEMENT_3D('',#9082,#6607,#6608);
#5634=AXIS2_PLACEMENT_3D('',#9084,#6609,#6610);
#5635=AXIS2_PLACEMENT_3D('',#9087,#6612,#6613);
#5636=AXIS2_PLACEMENT_3D('',#9088,#6614,#6615);
#5637=AXIS2_PLACEMENT_3D('',#9089,#6616,#6617);
#5638=AXIS2_PLACEMENT_3D('',#9090,#6618,#6619);
#5639=AXIS2_PLACEMENT_3D('',#9091,#6620,#6621);
#5640=AXIS2_PLACEMENT_3D('',#9093,#6622,#6623);
#5641=AXIS2_PLACEMENT_3D('',#9096,#6625,#6626);
#5642=AXIS2_PLACEMENT_3D('',#9097,#6627,#6628);
#5643=AXIS2_PLACEMENT_3D('',#9099,#6629,#6630);
#5644=AXIS2_PLACEMENT_3D('',#9102,#6632,#6633);
#5645=AXIS2_PLACEMENT_3D('',#9103,#6634,#6635);
#5646=AXIS2_PLACEMENT_3D('',#9104,#6636,#6637);
#5647=AXIS2_PLACEMENT_3D('',#9105,#6638,#6639);
#5648=AXIS2_PLACEMENT_3D('',#9106,#6640,#6641);
#5649=AXIS2_PLACEMENT_3D('',#9110,#6643,#6644);
#5650=AXIS2_PLACEMENT_3D('',#9111,#6645,#6646);
#5651=AXIS2_PLACEMENT_3D('',#9113,#6647,#6648);
#5652=AXIS2_PLACEMENT_3D('',#9157,#6652,#6653);
#5653=AXIS2_PLACEMENT_3D('',#9159,#6654,#6655);
#5654=AXIS2_PLACEMENT_3D('',#9160,#6656,#6657);
#5655=AXIS2_PLACEMENT_3D('',#9161,#6658,#6659);
#5656=AXIS2_PLACEMENT_3D('',#9164,#6661,#6662);
#5657=AXIS2_PLACEMENT_3D('',#9165,#6663,#6664);
#5658=AXIS2_PLACEMENT_3D('',#9167,#6665,#6666);
#5659=AXIS2_PLACEMENT_3D('',#9170,#6668,#6669);
#5660=AXIS2_PLACEMENT_3D('',#9171,#6670,#6671);
#5661=AXIS2_PLACEMENT_3D('',#9172,#6672,#6673);
#5662=AXIS2_PLACEMENT_3D('',#9174,#6674,#6675);
#5663=AXIS2_PLACEMENT_3D('',#9211,#6677,#6678);
#5664=AXIS2_PLACEMENT_3D('',#9212,#6679,#6680);
#5665=AXIS2_PLACEMENT_3D('',#9214,#6681,#6682);
#5666=AXIS2_PLACEMENT_3D('',#9217,#6684,#6685);
#5667=AXIS2_PLACEMENT_3D('',#9218,#6686,#6687);
#5668=AXIS2_PLACEMENT_3D('',#9220,#6688,#6689);
#5669=AXIS2_PLACEMENT_3D('',#9221,#6690,#6691);
#5670=AXIS2_PLACEMENT_3D('',#9223,#6692,#6693);
#5671=AXIS2_PLACEMENT_3D('',#9224,#6694,#6695);
#5672=AXIS2_PLACEMENT_3D('',#9226,#6696,#6697);
#5673=AXIS2_PLACEMENT_3D('',#9228,#6699,#6700);
#5674=AXIS2_PLACEMENT_3D('',#9231,#6702,#6703);
#5675=AXIS2_PLACEMENT_3D('',#9232,#6704,#6705);
#5676=AXIS2_PLACEMENT_3D('',#9234,#6706,#6707);
#5677=AXIS2_PLACEMENT_3D('',#9237,#6709,#6710);
#5678=AXIS2_PLACEMENT_3D('',#9238,#6711,#6712);
#5679=AXIS2_PLACEMENT_3D('',#9240,#6713,#6714);
#5680=AXIS2_PLACEMENT_3D('',#9241,#6715,#6716);
#5681=AXIS2_PLACEMENT_3D('',#9244,#6718,#6719);
#5682=AXIS2_PLACEMENT_3D('',#9245,#6720,#6721);
#5683=AXIS2_PLACEMENT_3D('',#9246,#6722,#6723);
#5684=AXIS2_PLACEMENT_3D('',#9248,#6724,#6725);
#5685=AXIS2_PLACEMENT_3D('',#9251,#6727,#6728);
#5686=AXIS2_PLACEMENT_3D('',#9252,#6729,#6730);
#5687=AXIS2_PLACEMENT_3D('',#9254,#6731,#6732);
#5688=AXIS2_PLACEMENT_3D('',#9257,#6734,#6735);
#5689=AXIS2_PLACEMENT_3D('',#9258,#6736,#6737);
#5690=AXIS2_PLACEMENT_3D('',#9260,#6738,#6739);
#5691=AXIS2_PLACEMENT_3D('',#9263,#6741,#6742);
#5692=AXIS2_PLACEMENT_3D('',#9264,#6743,#6744);
#5693=AXIS2_PLACEMENT_3D('',#9266,#6745,#6746);
#5694=AXIS2_PLACEMENT_3D('',#9269,#6748,#6749);
#5695=AXIS2_PLACEMENT_3D('',#9270,#6750,#6751);
#5696=AXIS2_PLACEMENT_3D('',#9272,#6752,#6753);
#5697=AXIS2_PLACEMENT_3D('',#9275,#6755,#6756);
#5698=AXIS2_PLACEMENT_3D('',#9276,#6757,#6758);
#5699=AXIS2_PLACEMENT_3D('',#9277,#6759,#6760);
#5700=AXIS2_PLACEMENT_3D('',#9278,#6761,#6762);
#5701=AXIS2_PLACEMENT_3D('',#9279,#6763,#6764);
#5702=AXIS2_PLACEMENT_3D('',#9281,#6765,#6766);
#5703=AXIS2_PLACEMENT_3D('',#9284,#6768,#6769);
#5704=AXIS2_PLACEMENT_3D('',#9285,#6770,#6771);
#5705=AXIS2_PLACEMENT_3D('',#9287,#6772,#6773);
#5706=AXIS2_PLACEMENT_3D('',#9290,#6775,#6776);
#5707=AXIS2_PLACEMENT_3D('',#9291,#6777,#6778);
#5708=AXIS2_PLACEMENT_3D('',#9292,#6779,#6780);
#5709=AXIS2_PLACEMENT_3D('',#9293,#6781,#6782);
#5710=AXIS2_PLACEMENT_3D('',#9294,#6783,#6784);
#5711=AXIS2_PLACEMENT_3D('',#9296,#6785,#6786);
#5712=AXIS2_PLACEMENT_3D('',#9299,#6788,#6789);
#5713=AXIS2_PLACEMENT_3D('',#9300,#6790,#6791);
#5714=AXIS2_PLACEMENT_3D('',#9302,#6792,#6793);
#5715=AXIS2_PLACEMENT_3D('',#9305,#6795,#6796);
#5716=AXIS2_PLACEMENT_3D('',#9306,#6797,#6798);
#5717=AXIS2_PLACEMENT_3D('',#9307,#6799,#6800);
#5718=AXIS2_PLACEMENT_3D('',#9308,#6801,#6802);
#5719=AXIS2_PLACEMENT_3D('',#9309,#6803,#6804);
#5720=AXIS2_PLACEMENT_3D('',#9311,#6805,#6806);
#5721=AXIS2_PLACEMENT_3D('',#9314,#6808,#6809);
#5722=AXIS2_PLACEMENT_3D('',#9315,#6810,#6811);
#5723=AXIS2_PLACEMENT_3D('',#9317,#6812,#6813);
#5724=AXIS2_PLACEMENT_3D('',#9320,#6815,#6816);
#5725=AXIS2_PLACEMENT_3D('',#9321,#6817,#6818);
#5726=AXIS2_PLACEMENT_3D('',#9322,#6819,#6820);
#5727=AXIS2_PLACEMENT_3D('',#9323,#6821,#6822);
#5728=AXIS2_PLACEMENT_3D('',#9324,#6823,#6824);
#5729=AXIS2_PLACEMENT_3D('',#9326,#6825,#6826);
#5730=AXIS2_PLACEMENT_3D('',#9329,#6828,#6829);
#5731=AXIS2_PLACEMENT_3D('',#9330,#6830,#6831);
#5732=AXIS2_PLACEMENT_3D('',#9331,#6832,#6833);
#5733=AXIS2_PLACEMENT_3D('',#9332,#6834,#6835);
#5734=AXIS2_PLACEMENT_3D('',#9333,#6836,#6837);
#5735=AXIS2_PLACEMENT_3D('',#9335,#6838,#6839);
#5736=AXIS2_PLACEMENT_3D('',#9338,#6841,#6842);
#5737=AXIS2_PLACEMENT_3D('',#9339,#6843,#6844);
#5738=AXIS2_PLACEMENT_3D('',#9340,#6845,#6846);
#5739=AXIS2_PLACEMENT_3D('',#9341,#6847,#6848);
#5740=AXIS2_PLACEMENT_3D('',#9342,#6849,#6850);
#5741=AXIS2_PLACEMENT_3D('',#9344,#6851,#6852);
#5742=AXIS2_PLACEMENT_3D('',#9347,#6854,#6855);
#5743=AXIS2_PLACEMENT_3D('',#9348,#6856,#6857);
#5744=AXIS2_PLACEMENT_3D('',#9349,#6858,#6859);
#5745=AXIS2_PLACEMENT_3D('',#9350,#6860,#6861);
#5746=AXIS2_PLACEMENT_3D('',#9351,#6862,#6863);
#5747=AXIS2_PLACEMENT_3D('',#9353,#6864,#6865);
#5748=AXIS2_PLACEMENT_3D('',#9356,#6867,#6868);
#5749=AXIS2_PLACEMENT_3D('',#9357,#6869,#6870);
#5750=AXIS2_PLACEMENT_3D('',#9358,#6871,#6872);
#5751=AXIS2_PLACEMENT_3D('',#9359,#6873,#6874);
#5752=AXIS2_PLACEMENT_3D('',#9360,#6875,#6876);
#5753=AXIS2_PLACEMENT_3D('',#9361,#6877,#6878);
#5754=AXIS2_PLACEMENT_3D('',#9364,#6879,#6880);
#5755=AXIS2_PLACEMENT_3D('',#9370,#6884,#6885);
#5756=AXIS2_PLACEMENT_3D('',#9376,#6889,#6890);
#5757=AXIS2_PLACEMENT_3D('',#9378,#6891,#6892);
#5758=AXIS2_PLACEMENT_3D('',#9382,#6895,#6896);
#5759=AXIS2_PLACEMENT_3D('',#9385,#6899,#6900);
#5760=AXIS2_PLACEMENT_3D('',#9386,#6901,#6902);
#5761=AXIS2_PLACEMENT_3D('',#9388,#6903,#6904);
#5762=AXIS2_PLACEMENT_3D('',#9390,#6905,#6906);
#5763=AXIS2_PLACEMENT_3D('',#9391,#6907,#6908);
#5764=AXIS2_PLACEMENT_3D('',#9393,#6909,#6910);
#5765=AXIS2_PLACEMENT_3D('',#9395,#6912,#6913);
#5766=AXIS2_PLACEMENT_3D('',#9397,#6914,#6915);
#5767=AXIS2_PLACEMENT_3D('',#9398,#6916,#6917);
#5768=AXIS2_PLACEMENT_3D('',#9400,#6918,#6919);
#5769=AXIS2_PLACEMENT_3D('',#9402,#6921,#6922);
#5770=AXIS2_PLACEMENT_3D('',#9404,#6923,#6924);
#5771=AXIS2_PLACEMENT_3D('',#9405,#6925,#6926);
#5772=AXIS2_PLACEMENT_3D('',#9407,#6927,#6928);
#5773=AXIS2_PLACEMENT_3D('',#9409,#6930,#6931);
#5774=AXIS2_PLACEMENT_3D('',#9411,#6932,#6933);
#5775=AXIS2_PLACEMENT_3D('',#9412,#6934,#6935);
#5776=AXIS2_PLACEMENT_3D('',#9414,#6936,#6937);
#5777=AXIS2_PLACEMENT_3D('',#9416,#6939,#6940);
#5778=AXIS2_PLACEMENT_3D('',#9418,#6941,#6942);
#5779=AXIS2_PLACEMENT_3D('',#9419,#6943,#6944);
#5780=AXIS2_PLACEMENT_3D('',#9421,#6945,#6946);
#5781=AXIS2_PLACEMENT_3D('',#9423,#6948,#6949);
#5782=AXIS2_PLACEMENT_3D('',#9425,#6950,#6951);
#5783=AXIS2_PLACEMENT_3D('',#9426,#6952,#6953);
#5784=AXIS2_PLACEMENT_3D('',#9428,#6955,#6956);
#5785=AXIS2_PLACEMENT_3D('',#9429,#6957,#6958);
#5786=AXIS2_PLACEMENT_3D('',#9432,#6959,#6960);
#5787=AXIS2_PLACEMENT_3D('',#9436,#6962,#6963);
#5788=AXIS2_PLACEMENT_3D('',#9438,#6965,#6966);
#5789=AXIS2_PLACEMENT_3D('',#9444,#6970,#6971);
#5790=AXIS2_PLACEMENT_3D('',#9446,#6972,#6973);
#5791=AXIS2_PLACEMENT_3D('',#9448,#6974,#6975);
#5792=AXIS2_PLACEMENT_3D('',#9450,#6977,#6978);
#5793=AXIS2_PLACEMENT_3D('',#9453,#6981,#6982);
#5794=AXIS2_PLACEMENT_3D('',#9455,#6983,#6984);
#5795=AXIS2_PLACEMENT_3D('',#9457,#6985,#6986);
#5796=AXIS2_PLACEMENT_3D('',#9458,#6987,#6988);
#5797=AXIS2_PLACEMENT_3D('',#9460,#6989,#6990);
#5798=AXIS2_PLACEMENT_3D('',#9462,#6992,#6993);
#5799=AXIS2_PLACEMENT_3D('',#9464,#6994,#6995);
#5800=AXIS2_PLACEMENT_3D('',#9465,#6996,#6997);
#5801=AXIS2_PLACEMENT_3D('',#9467,#6999,#7000);
#5802=AXIS2_PLACEMENT_3D('',#9468,#7001,#7002);
#5803=AXIS2_PLACEMENT_3D('',#9469,#7003,#7004);
#5804=AXIS2_PLACEMENT_3D('',#9470,#7005,#7006);
#5805=AXIS2_PLACEMENT_3D('',#9472,#7007,#7008);
#5806=AXIS2_PLACEMENT_3D('',#9473,#7009,#7010);
#5807=AXIS2_PLACEMENT_3D('',#9475,#7011,#7012);
#5808=AXIS2_PLACEMENT_3D('',#9477,#7014,#7015);
#5809=AXIS2_PLACEMENT_3D('',#9479,#7016,#7017);
#5810=AXIS2_PLACEMENT_3D('',#9481,#7019,#7020);
#5811=AXIS2_PLACEMENT_3D('',#9483,#7021,#7022);
#5812=AXIS2_PLACEMENT_3D('',#9485,#7024,#7025);
#5813=AXIS2_PLACEMENT_3D('',#9487,#7026,#7027);
#5814=AXIS2_PLACEMENT_3D('',#9488,#7028,#7029);
#5815=AXIS2_PLACEMENT_3D('',#9490,#7030,#7031);
#5816=AXIS2_PLACEMENT_3D('',#9492,#7033,#7034);
#5817=AXIS2_PLACEMENT_3D('',#9494,#7035,#7036);
#5818=AXIS2_PLACEMENT_3D('',#9496,#7038,#7039);
#5819=AXIS2_PLACEMENT_3D('',#9498,#7040,#7041);
#5820=AXIS2_PLACEMENT_3D('',#9500,#7043,#7044);
#5821=AXIS2_PLACEMENT_3D('',#9501,#7045,#7046);
#5822=AXIS2_PLACEMENT_3D('',#9510,#7051,#7052);
#5823=AXIS2_PLACEMENT_3D('',#9516,#7056,#7057);
#5824=AXIS2_PLACEMENT_3D('',#9522,#7061,#7062);
#5825=AXIS2_PLACEMENT_3D('',#9528,#7066,#7067);
#5826=AXIS2_PLACEMENT_3D('',#9534,#7071,#7072);
#5827=AXIS2_PLACEMENT_3D('',#9537,#7075,#7076);
#5828=AXIS2_PLACEMENT_3D('',#9538,#7077,#7078);
#5829=AXIS2_PLACEMENT_3D('',#9539,#7079,#7080);
#5830=AXIS2_PLACEMENT_3D('',#9540,#7081,#7082);
#5831=AXIS2_PLACEMENT_3D('',#9541,#7083,#7084);
#5832=AXIS2_PLACEMENT_3D('',#9543,#7085,#7086);
#5833=AXIS2_PLACEMENT_3D('',#9546,#7088,#7089);
#5834=AXIS2_PLACEMENT_3D('',#9547,#7090,#7091);
#5835=AXIS2_PLACEMENT_3D('',#9549,#7092,#7093);
#5836=AXIS2_PLACEMENT_3D('',#9550,#7094,#7095);
#5837=AXIS2_PLACEMENT_3D('',#9564,#7102,#7103);
#5838=AXIS2_PLACEMENT_3D('',#9565,#7104,#7105);
#5839=AXIS2_PLACEMENT_3D('',#9579,#7112,#7113);
#5840=AXIS2_PLACEMENT_3D('',#9580,#7114,#7115);
#5841=AXIS2_PLACEMENT_3D('',#9583,#7118,#7119);
#5842=AXIS2_PLACEMENT_3D('',#9585,#7121,#7122);
#5843=AXIS2_PLACEMENT_3D('',#9587,#7124,#7125);
#5844=AXIS2_PLACEMENT_3D('',#9589,#7127,#7128);
#5845=AXIS2_PLACEMENT_3D('',#9591,#7130,#7131);
#5846=AXIS2_PLACEMENT_3D('',#9592,#7132,#7133);
#5847=AXIS2_PLACEMENT_3D('',#9594,#7134,#7135);
#5848=AXIS2_PLACEMENT_3D('',#9595,#7136,#7137);
#5849=AXIS2_PLACEMENT_3D('',#9598,#7139,#7140);
#5850=AXIS2_PLACEMENT_3D('',#9599,#7141,#7142);
#5851=AXIS2_PLACEMENT_3D('',#9601,#7143,#7144);
#5852=AXIS2_PLACEMENT_3D('',#9602,#7145,#7146);
#5853=AXIS2_PLACEMENT_3D('',#9604,#7148,#7149);
#5854=AXIS2_PLACEMENT_3D('',#9606,#7150,#7151);
#5855=AXIS2_PLACEMENT_3D('',#9608,#7153,#7154);
#5856=AXIS2_PLACEMENT_3D('',#9610,#7155,#7156);
#5857=AXIS2_PLACEMENT_3D('',#9611,#7157,#7158);
#5858=AXIS2_PLACEMENT_3D('',#9613,#7160,#7161);
#5859=AXIS2_PLACEMENT_3D('',#9614,#7162,#7163);
#5860=AXIS2_PLACEMENT_3D('',#9616,#7164,#7165);
#5861=AXIS2_PLACEMENT_3D('',#9618,#7166,#7167);
#5862=AXIS2_PLACEMENT_3D('',#9619,#7168,#7169);
#5863=AXIS2_PLACEMENT_3D('',#9621,#7170,#7171);
#5864=AXIS2_PLACEMENT_3D('',#9623,#7173,#7174);
#5865=AXIS2_PLACEMENT_3D('',#9625,#7175,#7176);
#5866=AXIS2_PLACEMENT_3D('',#9626,#7177,#7178);
#5867=AXIS2_PLACEMENT_3D('',#9628,#7179,#7180);
#5868=AXIS2_PLACEMENT_3D('',#9630,#7182,#7183);
#5869=AXIS2_PLACEMENT_3D('',#9632,#7184,#7185);
#5870=AXIS2_PLACEMENT_3D('',#9633,#7186,#7187);
#5871=AXIS2_PLACEMENT_3D('',#9635,#7189,#7190);
#5872=AXIS2_PLACEMENT_3D('',#9636,#7191,#7192);
#5873=AXIS2_PLACEMENT_3D('',#9637,#7193,#7194);
#5874=AXIS2_PLACEMENT_3D('',#9638,#7195,#7196);
#5875=AXIS2_PLACEMENT_3D('',#9640,#7197,#7198);
#5876=AXIS2_PLACEMENT_3D('',#9643,#7200,#7201);
#5877=AXIS2_PLACEMENT_3D('',#9644,#7202,#7203);
#5878=AXIS2_PLACEMENT_3D('',#9647,#7205,#7206);
#5879=AXIS2_PLACEMENT_3D('',#9648,#7207,#7208);
#5880=AXIS2_PLACEMENT_3D('',#9650,#7209,#7210);
#5881=AXIS2_PLACEMENT_3D('',#9651,#7211,#7212);
#5882=AXIS2_PLACEMENT_3D('',#9654,#7214,#7215);
#5883=AXIS2_PLACEMENT_3D('',#9655,#7216,#7217);
#5884=AXIS2_PLACEMENT_3D('',#9656,#7218,#7219);
#5885=AXIS2_PLACEMENT_3D('',#9657,#7220,#7221);
#5886=AXIS2_PLACEMENT_3D('',#9669,#7223,#7224);
#5887=AXIS2_PLACEMENT_3D('',#9685,#7225,#7226);
#5888=AXIS2_PLACEMENT_3D('',#9687,#7227,#7228);
#5889=AXIS2_PLACEMENT_3D('',#9713,#7230,#7231);
#5890=AXIS2_PLACEMENT_3D('',#9716,#7234,#7235);
#5891=AXIS2_PLACEMENT_3D('',#9718,#7237,#7238);
#5892=AXIS2_PLACEMENT_3D('',#9720,#7240,#7241);
#5893=AXIS2_PLACEMENT_3D('',#9722,#7242,#7243);
#5894=AXIS2_PLACEMENT_3D('',#9725,#7245,#7246);
#5895=AXIS2_PLACEMENT_3D('',#9726,#7247,#7248);
#5896=AXIS2_PLACEMENT_3D('',#9728,#7250,#7251);
#5897=AXIS2_PLACEMENT_3D('',#9730,#7253,#7254);
#5898=AXIS2_PLACEMENT_3D('',#9731,#7255,#7256);
#5899=AXIS2_PLACEMENT_3D('',#9732,#7257,#7258);
#5900=AXIS2_PLACEMENT_3D('',#9733,#7259,#7260);
#5901=AXIS2_PLACEMENT_3D('',#9734,#7261,#7262);
#5902=AXIS2_PLACEMENT_3D('',#9735,#7263,#7264);
#5903=AXIS2_PLACEMENT_3D('',#9737,#7265,#7266);
#5904=AXIS2_PLACEMENT_3D('',#9740,#7268,#7269);
#5905=AXIS2_PLACEMENT_3D('',#9741,#7270,#7271);
#5906=AXIS2_PLACEMENT_3D('',#9743,#7272,#7273);
#5907=AXIS2_PLACEMENT_3D('',#9744,#7274,#7275);
#5908=AXIS2_PLACEMENT_3D('',#9746,#7276,#7277);
#5909=AXIS2_PLACEMENT_3D('',#9748,#7279,#7280);
#5910=AXIS2_PLACEMENT_3D('',#9757,#7285,#7286);
#5911=AXIS2_PLACEMENT_3D('',#9763,#7290,#7291);
#5912=AXIS2_PLACEMENT_3D('',#9769,#7295,#7296);
#5913=AXIS2_PLACEMENT_3D('',#9775,#7300,#7301);
#5914=AXIS2_PLACEMENT_3D('',#9779,#7304,#7305);
#5915=AXIS2_PLACEMENT_3D('',#9787,#7310,#7311);
#5916=AXIS2_PLACEMENT_3D('',#9805,#7321,#7322);
#5917=AXIS2_PLACEMENT_3D('',#9809,#7324,#7325);
#5918=AXIS2_PLACEMENT_3D('',#9810,#7326,#7327);
#5919=AXIS2_PLACEMENT_3D('',#9827,#7328,#7329);
#5920=AXIS2_PLACEMENT_3D('',#9884,#7331,#7332);
#5921=AXIS2_PLACEMENT_3D('',#9886,#7334,#7335);
#5922=AXIS2_PLACEMENT_3D('',#9888,#7336,#7337);
#5923=AXIS2_PLACEMENT_3D('',#9892,#7339,#7340);
#5924=AXIS2_PLACEMENT_3D('',#9893,#7341,#7342);
#5925=AXIS2_PLACEMENT_3D('',#9894,#7343,#7344);
#5926=AXIS2_PLACEMENT_3D('',#9896,#7345,#7346);
#5927=AXIS2_PLACEMENT_3D('',#9901,#7349,#7350);
#5928=AXIS2_PLACEMENT_3D('',#9903,#7352,#7353);
#5929=AXIS2_PLACEMENT_3D('',#9904,#7354,#7355);
#5930=AXIS2_PLACEMENT_3D('',#9915,#7362,#7363);
#5931=AXIS2_PLACEMENT_3D('',#9916,#7364,#7365);
#5932=AXIS2_PLACEMENT_3D('',#9917,#7366,#7367);
#5933=AXIS2_PLACEMENT_3D('',#9918,#7368,#7369);
#5934=AXIS2_PLACEMENT_3D('',#9919,#7370,#7371);
#5935=AXIS2_PLACEMENT_3D('',#9921,#7372,#7373);
#5936=AXIS2_PLACEMENT_3D('',#9922,#7374,#7375);
#5937=AXIS2_PLACEMENT_3D('',#9923,#7376,#7377);
#5938=AXIS2_PLACEMENT_3D('',#9926,#7379,#7380);
#5939=AXIS2_PLACEMENT_3D('',#9927,#7381,#7382);
#5940=AXIS2_PLACEMENT_3D('',#9928,#7383,#7384);
#5941=AXIS2_PLACEMENT_3D('',#9930,#7386,#7387);
#5942=AXIS2_PLACEMENT_3D('',#9931,#7388,#7389);
#5943=AXIS2_PLACEMENT_3D('',#9933,#7391,#7392);
#5944=AXIS2_PLACEMENT_3D('',#9934,#7393,#7394);
#5945=AXIS2_PLACEMENT_3D('',#9935,#7395,#7396);
#5946=AXIS2_PLACEMENT_3D('',#9937,#7397,#7398);
#5947=AXIS2_PLACEMENT_3D('',#9940,#7400,#7401);
#5948=AXIS2_PLACEMENT_3D('',#9941,#7402,#7403);
#5949=AXIS2_PLACEMENT_3D('',#9942,#7404,#7405);
#5950=AXIS2_PLACEMENT_3D('',#9944,#7406,#7407);
#5951=AXIS2_PLACEMENT_3D('',#9947,#7409,#7410);
#5952=AXIS2_PLACEMENT_3D('',#9948,#7411,#7412);
#5953=AXIS2_PLACEMENT_3D('',#9949,#7413,#7414);
#5954=AXIS2_PLACEMENT_3D('',#9951,#7415,#7416);
#5955=AXIS2_PLACEMENT_3D('',#9954,#7418,#7419);
#5956=AXIS2_PLACEMENT_3D('',#9955,#7420,#7421);
#5957=AXIS2_PLACEMENT_3D('',#9956,#7422,#7423);
#5958=AXIS2_PLACEMENT_3D('',#9957,#7424,#7425);
#5959=AXIS2_PLACEMENT_3D('',#9958,#7426,#7427);
#5960=AXIS2_PLACEMENT_3D('',#9960,#7428,#7429);
#5961=AXIS2_PLACEMENT_3D('',#9963,#7431,#7432);
#5962=AXIS2_PLACEMENT_3D('',#9964,#7433,#7434);
#5963=AXIS2_PLACEMENT_3D('',#9966,#7435,#7436);
#5964=AXIS2_PLACEMENT_3D('',#9967,#7437,#7438);
#5965=AXIS2_PLACEMENT_3D('',#9969,#7439,#7440);
#5966=AXIS2_PLACEMENT_3D('',#9970,#7441,#7442);
#5967=AXIS2_PLACEMENT_3D('',#9973,#7444,#7445);
#5968=AXIS2_PLACEMENT_3D('',#9974,#7446,#7447);
#5969=AXIS2_PLACEMENT_3D('',#9976,#7448,#7449);
#5970=AXIS2_PLACEMENT_3D('',#9979,#7451,#7452);
#5971=AXIS2_PLACEMENT_3D('',#9980,#7453,#7454);
#5972=AXIS2_PLACEMENT_3D('',#9982,#7455,#7456);
#5973=AXIS2_PLACEMENT_3D('',#9984,#7458,#7459);
#5974=AXIS2_PLACEMENT_3D('',#9985,#7460,#7461);
#5975=AXIS2_PLACEMENT_3D('',#9986,#7462,#7463);
#5976=AXIS2_PLACEMENT_3D('',#9987,#7464,#7465);
#5977=AXIS2_PLACEMENT_3D('',#9989,#7466,#7467);
#5978=AXIS2_PLACEMENT_3D('',#9992,#7469,#7470);
#5979=AXIS2_PLACEMENT_3D('',#9993,#7471,#7472);
#5980=AXIS2_PLACEMENT_3D('',#9995,#7473,#7474);
#5981=AXIS2_PLACEMENT_3D('',#9998,#7476,#7477);
#5982=AXIS2_PLACEMENT_3D('',#9999,#7478,#7479);
#5983=AXIS2_PLACEMENT_3D('',#10000,#7480,#7481);
#5984=AXIS2_PLACEMENT_3D('',#10001,#7482,#7483);
#5985=AXIS2_PLACEMENT_3D('',#10002,#7484,#7485);
#5986=AXIS2_PLACEMENT_3D('',#10004,#7486,#7487);
#5987=AXIS2_PLACEMENT_3D('',#10005,#7488,#7489);
#5988=AXIS2_PLACEMENT_3D('',#10007,#7490,#7491);
#5989=AXIS2_PLACEMENT_3D('',#10010,#7493,#7494);
#5990=AXIS2_PLACEMENT_3D('',#10011,#7495,#7496);
#5991=AXIS2_PLACEMENT_3D('',#10013,#7498,#7499);
#5992=AXIS2_PLACEMENT_3D('',#10014,#7500,#7501);
#5993=AXIS2_PLACEMENT_3D('',#10015,#7502,#7503);
#5994=AXIS2_PLACEMENT_3D('',#10017,#7504,#7505);
#5995=AXIS2_PLACEMENT_3D('',#10018,#7506,#7507);
#5996=AXIS2_PLACEMENT_3D('',#10027,#7512,#7513);
#5997=AXIS2_PLACEMENT_3D('',#10033,#7517,#7518);
#5998=AXIS2_PLACEMENT_3D('',#10039,#7522,#7523);
#5999=AXIS2_PLACEMENT_3D('',#10045,#7527,#7528);
#6000=AXIS2_PLACEMENT_3D('',#10051,#7532,#7533);
#6001=AXIS2_PLACEMENT_3D('',#10054,#7536,#7537);
#6002=AXIS2_PLACEMENT_3D('',#10055,#7538,#7539);
#6003=AXIS2_PLACEMENT_3D('',#10057,#7540,#7541);
#6004=AXIS2_PLACEMENT_3D('',#10058,#7542,#7543);
#6005=AXIS2_PLACEMENT_3D('',#10060,#7544,#7545);
#6006=AXIS2_PLACEMENT_3D('',#10062,#7547,#7548);
#6007=AXIS2_PLACEMENT_3D('',#10064,#7550,#7551);
#6008=AXIS2_PLACEMENT_3D('',#10065,#7552,#7553);
#6009=AXIS2_PLACEMENT_3D('',#10067,#7554,#7555);
#6010=AXIS2_PLACEMENT_3D('',#10068,#7556,#7557);
#6011=AXIS2_PLACEMENT_3D('',#10070,#7558,#7559);
#6012=AXIS2_PLACEMENT_3D('',#10072,#7561,#7562);
#6013=AXIS2_PLACEMENT_3D('',#10074,#7563,#7564);
#6014=AXIS2_PLACEMENT_3D('',#10076,#7566,#7567);
#6015=AXIS2_PLACEMENT_3D('',#10078,#7568,#7569);
#6016=AXIS2_PLACEMENT_3D('',#10080,#7571,#7572);
#6017=AXIS2_PLACEMENT_3D('',#10082,#7573,#7574);
#6018=AXIS2_PLACEMENT_3D('',#10083,#7575,#7576);
#6019=AXIS2_PLACEMENT_3D('',#10085,#7577,#7578);
#6020=AXIS2_PLACEMENT_3D('',#10087,#7580,#7581);
#6021=AXIS2_PLACEMENT_3D('',#10089,#7582,#7583);
#6022=AXIS2_PLACEMENT_3D('',#10091,#7585,#7586);
#6023=AXIS2_PLACEMENT_3D('',#10093,#7587,#7588);
#6024=AXIS2_PLACEMENT_3D('',#10095,#7590,#7591);
#6025=AXIS2_PLACEMENT_3D('',#10096,#7592,#7593);
#6026=AXIS2_PLACEMENT_3D('',#10105,#7598,#7599);
#6027=AXIS2_PLACEMENT_3D('',#10111,#7603,#7604);
#6028=AXIS2_PLACEMENT_3D('',#10117,#7608,#7609);
#6029=AXIS2_PLACEMENT_3D('',#10123,#7613,#7614);
#6030=AXIS2_PLACEMENT_3D('',#10129,#7618,#7619);
#6031=AXIS2_PLACEMENT_3D('',#10132,#7622,#7623);
#6032=AXIS2_PLACEMENT_3D('',#10133,#7624,#7625);
#6033=AXIS2_PLACEMENT_3D('',#10134,#7626,#7627);
#6034=AXIS2_PLACEMENT_3D('',#10135,#7628,#7629);
#6035=AXIS2_PLACEMENT_3D('',#10136,#7630,#7631);
#6036=AXIS2_PLACEMENT_3D('',#10137,#7632,#7633);
#6037=AXIS2_PLACEMENT_3D('',#10138,#7634,#7635);
#6038=AXIS2_PLACEMENT_3D('',#10139,#7636,#7637);
#6039=AXIS2_PLACEMENT_3D('',#10140,#7638,#7639);
#6040=AXIS2_PLACEMENT_3D('',#10141,#7640,#7641);
#6041=AXIS2_PLACEMENT_3D('',#10142,#7642,#7643);
#6042=AXIS2_PLACEMENT_3D('',#10143,#7644,#7645);
#6043=AXIS2_PLACEMENT_3D('',#10144,#7646,#7647);
#6044=AXIS2_PLACEMENT_3D('',#10145,#7648,#7649);
#6045=AXIS2_PLACEMENT_3D('',#10146,#7650,#7651);
#6046=AXIS2_PLACEMENT_3D('',#10147,#7652,#7653);
#6047=AXIS2_PLACEMENT_3D('',#10148,#7654,#7655);
#6048=AXIS2_PLACEMENT_3D('',#10149,#7656,#7657);
#6049=AXIS2_PLACEMENT_3D('',#10150,#7658,#7659);
#6050=AXIS2_PLACEMENT_3D('',#10151,#7660,#7661);
#6051=AXIS2_PLACEMENT_3D('',#10152,#7662,#7663);
#6052=AXIS2_PLACEMENT_3D('',#10153,#7664,#7665);
#6053=AXIS2_PLACEMENT_3D('',#10154,#7666,#7667);
#6054=AXIS2_PLACEMENT_3D('',#10155,#7668,#7669);
#6055=AXIS2_PLACEMENT_3D('',#10156,#7670,#7671);
#6056=AXIS2_PLACEMENT_3D('',#10157,#7672,#7673);
#6057=AXIS2_PLACEMENT_3D('',#10158,#7674,#7675);
#6058=AXIS2_PLACEMENT_3D('',#10159,#7676,#7677);
#6059=AXIS2_PLACEMENT_3D('',#10160,#7678,#7679);
#6060=AXIS2_PLACEMENT_3D('',#10161,#7680,#7681);
#6061=AXIS2_PLACEMENT_3D('',#10162,#7682,#7683);
#6062=AXIS2_PLACEMENT_3D('',#10163,#7684,#7685);
#6063=AXIS2_PLACEMENT_3D('',#10164,#7686,#7687);
#6064=AXIS2_PLACEMENT_3D('',#10165,#7688,#7689);
#6065=AXIS2_PLACEMENT_3D('',#10166,#7690,#7691);
#6066=AXIS2_PLACEMENT_3D('',#10167,#7692,#7693);
#6067=AXIS2_PLACEMENT_3D('',#10168,#7694,#7695);
#6068=AXIS2_PLACEMENT_3D('',#10169,#7696,#7697);
#6069=AXIS2_PLACEMENT_3D('',#10170,#7698,#7699);
#6070=AXIS2_PLACEMENT_3D('',#10171,#7700,#7701);
#6071=AXIS2_PLACEMENT_3D('',#10172,#7702,#7703);
#6072=AXIS2_PLACEMENT_3D('',#10173,#7704,#7705);
#6073=AXIS2_PLACEMENT_3D('',#10174,#7706,#7707);
#6074=AXIS2_PLACEMENT_3D('',#10175,#7708,#7709);
#6075=AXIS2_PLACEMENT_3D('',#10176,#7710,#7711);
#6076=AXIS2_PLACEMENT_3D('',#10177,#7712,#7713);
#6077=AXIS2_PLACEMENT_3D('',#10178,#7714,#7715);
#6078=AXIS2_PLACEMENT_3D('',#10179,#7716,#7717);
#6079=AXIS2_PLACEMENT_3D('',#10180,#7718,#7719);
#6080=AXIS2_PLACEMENT_3D('',#10181,#7720,#7721);
#6081=AXIS2_PLACEMENT_3D('',#10182,#7722,#7723);
#6082=AXIS2_PLACEMENT_3D('',#10183,#7724,#7725);
#6083=AXIS2_PLACEMENT_3D('',#10184,#7726,#7727);
#6084=AXIS2_PLACEMENT_3D('',#10185,#7728,#7729);
#6085=AXIS2_PLACEMENT_3D('',#10186,#7730,#7731);
#6086=AXIS2_PLACEMENT_3D('',#10187,#7732,#7733);
#6087=AXIS2_PLACEMENT_3D('',#10188,#7734,#7735);
#6088=AXIS2_PLACEMENT_3D('',#10189,#7736,#7737);
#6089=DIRECTION('axis',(0.,0.,1.));
#6090=DIRECTION('refdir',(1.,0.,0.));
#6091=DIRECTION('axis',(0.,0.,1.));
#6092=DIRECTION('refdir',(1.,0.,0.));
#6093=DIRECTION('axis',(0.,0.,1.));
#6094=DIRECTION('refdir',(1.,0.,0.));
#6095=DIRECTION('center_axis',(0.,0.,1.));
#6096=DIRECTION('ref_axis',(1.,0.,0.));
#6097=DIRECTION('center_axis',(0.,0.,1.));
#6098=DIRECTION('ref_axis',(1.,0.,0.));
#6099=DIRECTION('',(0.,0.,1.));
#6100=DIRECTION('center_axis',(0.,0.,-1.));
#6101=DIRECTION('ref_axis',(1.,0.,0.));
#6102=DIRECTION('center_axis',(0.,0.,1.));
#6103=DIRECTION('ref_axis',(1.,0.,0.));
#6104=DIRECTION('center_axis',(0.,0.,1.));
#6105=DIRECTION('ref_axis',(1.,0.,0.));
#6106=DIRECTION('',(0.,0.,1.));
#6107=DIRECTION('center_axis',(0.,0.,-1.));
#6108=DIRECTION('ref_axis',(1.,0.,0.));
#6109=DIRECTION('center_axis',(0.,0.,1.));
#6110=DIRECTION('ref_axis',(1.,0.,0.));
#6111=DIRECTION('center_axis',(0.,0.,1.));
#6112=DIRECTION('ref_axis',(1.,0.,0.));
#6113=DIRECTION('',(0.,0.,1.));
#6114=DIRECTION('center_axis',(0.,0.,-1.));
#6115=DIRECTION('ref_axis',(1.,0.,0.));
#6116=DIRECTION('center_axis',(0.,0.,1.));
#6117=DIRECTION('ref_axis',(1.,0.,0.));
#6118=DIRECTION('center_axis',(0.,0.,1.));
#6119=DIRECTION('ref_axis',(1.,0.,0.));
#6120=DIRECTION('',(0.,0.,1.));
#6121=DIRECTION('center_axis',(0.,0.,-1.));
#6122=DIRECTION('ref_axis',(1.,0.,0.));
#6123=DIRECTION('center_axis',(0.,0.,1.));
#6124=DIRECTION('ref_axis',(1.,0.,0.));
#6125=DIRECTION('center_axis',(0.,0.,1.));
#6126=DIRECTION('ref_axis',(1.,0.,0.));
#6127=DIRECTION('',(0.,0.,1.));
#6128=DIRECTION('center_axis',(0.,0.,-1.));
#6129=DIRECTION('ref_axis',(1.,0.,0.));
#6130=DIRECTION('center_axis',(0.,0.,1.));
#6131=DIRECTION('ref_axis',(1.,0.,0.));
#6132=DIRECTION('center_axis',(0.,0.,1.));
#6133=DIRECTION('ref_axis',(1.,0.,0.));
#6134=DIRECTION('',(0.,0.,1.));
#6135=DIRECTION('center_axis',(0.,0.,-1.));
#6136=DIRECTION('ref_axis',(1.,0.,0.));
#6137=DIRECTION('center_axis',(0.,0.,1.));
#6138=DIRECTION('ref_axis',(1.,0.,0.));
#6139=DIRECTION('center_axis',(0.,0.,1.));
#6140=DIRECTION('ref_axis',(1.,0.,0.));
#6141=DIRECTION('',(0.,0.,1.));
#6142=DIRECTION('center_axis',(0.,0.,-1.));
#6143=DIRECTION('ref_axis',(1.,0.,0.));
#6144=DIRECTION('center_axis',(0.,0.,1.));
#6145=DIRECTION('ref_axis',(1.,0.,0.));
#6146=DIRECTION('center_axis',(0.,0.,1.));
#6147=DIRECTION('ref_axis',(1.,0.,0.));
#6148=DIRECTION('',(0.,0.,1.));
#6149=DIRECTION('center_axis',(0.,0.,-1.));
#6150=DIRECTION('ref_axis',(1.,0.,0.));
#6151=DIRECTION('center_axis',(0.,0.,1.));
#6152=DIRECTION('ref_axis',(1.,0.,0.));
#6153=DIRECTION('center_axis',(0.,0.,1.));
#6154=DIRECTION('ref_axis',(1.,0.,0.));
#6155=DIRECTION('',(0.,0.,1.));
#6156=DIRECTION('center_axis',(0.,0.,-1.));
#6157=DIRECTION('ref_axis',(1.,0.,0.));
#6158=DIRECTION('center_axis',(0.,1.,0.));
#6159=DIRECTION('ref_axis',(-1.,0.,0.));
#6160=DIRECTION('',(-1.,0.,0.));
#6161=DIRECTION('',(0.,0.,1.));
#6162=DIRECTION('',(-1.,0.,0.));
#6163=DIRECTION('',(0.,0.,1.));
#6164=DIRECTION('center_axis',(1.,0.,0.));
#6165=DIRECTION('ref_axis',(0.,1.,0.));
#6166=DIRECTION('',(0.,1.,0.));
#6167=DIRECTION('',(0.,1.,0.));
#6168=DIRECTION('',(0.,0.,1.));
#6169=DIRECTION('center_axis',(0.,-1.,0.));
#6170=DIRECTION('ref_axis',(1.,0.,0.));
#6171=DIRECTION('',(1.,0.,0.));
#6172=DIRECTION('',(1.,0.,0.));
#6173=DIRECTION('',(0.,0.,1.));
#6174=DIRECTION('center_axis',(-1.,0.,0.));
#6175=DIRECTION('ref_axis',(0.,-1.,0.));
#6176=DIRECTION('',(0.,-1.,0.));
#6177=DIRECTION('',(0.,-1.,0.));
#6178=DIRECTION('center_axis',(0.,0.,1.));
#6179=DIRECTION('ref_axis',(1.,0.,0.));
#6180=DIRECTION('center_axis',(0.,0.,1.));
#6181=DIRECTION('ref_axis',(1.,0.,0.));
#6182=DIRECTION('axis',(0.,0.,1.));
#6183=DIRECTION('refdir',(1.,0.,0.));
#6184=DIRECTION('center_axis',(0.,1.,0.));
#6185=DIRECTION('ref_axis',(-1.,0.,0.));
#6186=DIRECTION('',(-1.,0.,0.));
#6187=DIRECTION('',(0.,0.,1.));
#6188=DIRECTION('',(-1.,0.,0.));
#6189=DIRECTION('',(0.,0.,1.));
#6190=DIRECTION('center_axis',(1.,0.,0.));
#6191=DIRECTION('ref_axis',(0.,1.,0.));
#6192=DIRECTION('',(0.,1.,0.));
#6193=DIRECTION('',(0.,1.,0.));
#6194=DIRECTION('',(0.,0.,1.));
#6195=DIRECTION('center_axis',(0.,-1.,0.));
#6196=DIRECTION('ref_axis',(1.,0.,0.));
#6197=DIRECTION('',(1.,0.,0.));
#6198=DIRECTION('',(1.,0.,0.));
#6199=DIRECTION('',(0.,0.,1.));
#6200=DIRECTION('center_axis',(-1.,0.,0.));
#6201=DIRECTION('ref_axis',(0.,-1.,0.));
#6202=DIRECTION('',(0.,-1.,0.));
#6203=DIRECTION('',(0.,-1.,0.));
#6204=DIRECTION('center_axis',(0.,0.,1.));
#6205=DIRECTION('ref_axis',(1.,0.,0.));
#6206=DIRECTION('center_axis',(0.,0.,1.));
#6207=DIRECTION('ref_axis',(1.,0.,0.));
#6208=DIRECTION('axis',(0.,0.,1.));
#6209=DIRECTION('refdir',(1.,0.,0.));
#6210=DIRECTION('center_axis',(0.,1.,0.));
#6211=DIRECTION('ref_axis',(-1.,0.,0.));
#6212=DIRECTION('',(-1.,0.,0.));
#6213=DIRECTION('',(0.,0.,1.));
#6214=DIRECTION('',(-1.,0.,0.));
#6215=DIRECTION('',(0.,0.,1.));
#6216=DIRECTION('center_axis',(1.,0.,0.));
#6217=DIRECTION('ref_axis',(0.,1.,0.));
#6218=DIRECTION('',(0.,1.,0.));
#6219=DIRECTION('',(0.,1.,0.));
#6220=DIRECTION('',(0.,0.,1.));
#6221=DIRECTION('center_axis',(0.,-1.,0.));
#6222=DIRECTION('ref_axis',(1.,0.,0.));
#6223=DIRECTION('',(1.,0.,0.));
#6224=DIRECTION('',(1.,0.,0.));
#6225=DIRECTION('',(0.,0.,1.));
#6226=DIRECTION('center_axis',(-1.,0.,0.));
#6227=DIRECTION('ref_axis',(0.,-1.,0.));
#6228=DIRECTION('',(0.,-1.,0.));
#6229=DIRECTION('',(0.,-1.,0.));
#6230=DIRECTION('center_axis',(0.,0.,1.));
#6231=DIRECTION('ref_axis',(1.,0.,0.));
#6232=DIRECTION('center_axis',(0.,0.,1.));
#6233=DIRECTION('ref_axis',(1.,0.,0.));
#6234=DIRECTION('axis',(0.,0.,1.));
#6235=DIRECTION('refdir',(1.,0.,0.));
#6236=DIRECTION('center_axis',(0.,0.,1.));
#6237=DIRECTION('ref_axis',(1.,0.,0.));
#6238=DIRECTION('center_axis',(0.,0.,1.));
#6239=DIRECTION('ref_axis',(1.,0.,0.));
#6240=DIRECTION('',(0.,0.,1.));
#6241=DIRECTION('center_axis',(0.,0.,-1.));
#6242=DIRECTION('ref_axis',(1.,0.,0.));
#6243=DIRECTION('center_axis',(0.,0.,1.));
#6244=DIRECTION('ref_axis',(1.,0.,0.));
#6245=DIRECTION('center_axis',(0.,0.,1.));
#6246=DIRECTION('ref_axis',(1.,0.,0.));
#6247=DIRECTION('center_axis',(0.,0.,1.));
#6248=DIRECTION('ref_axis',(1.,0.,0.));
#6249=DIRECTION('',(0.,0.,1.));
#6250=DIRECTION('center_axis',(0.,0.,-1.));
#6251=DIRECTION('ref_axis',(1.,0.,0.));
#6252=DIRECTION('center_axis',(0.,0.,1.));
#6253=DIRECTION('ref_axis',(1.,0.,0.));
#6254=DIRECTION('center_axis',(0.,0.,1.));
#6255=DIRECTION('ref_axis',(1.,0.,0.));
#6256=DIRECTION('center_axis',(0.,0.,1.));
#6257=DIRECTION('ref_axis',(1.,0.,0.));
#6258=DIRECTION('',(0.,0.,1.));
#6259=DIRECTION('center_axis',(0.,0.,-1.));
#6260=DIRECTION('ref_axis',(1.,0.,0.));
#6261=DIRECTION('center_axis',(0.,0.,1.));
#6262=DIRECTION('ref_axis',(1.,0.,0.));
#6263=DIRECTION('center_axis',(0.,0.,1.));
#6264=DIRECTION('ref_axis',(1.,0.,0.));
#6265=DIRECTION('center_axis',(0.,0.,1.));
#6266=DIRECTION('ref_axis',(1.,0.,0.));
#6267=DIRECTION('',(0.,0.,1.));
#6268=DIRECTION('center_axis',(0.,0.,-1.));
#6269=DIRECTION('ref_axis',(1.,0.,0.));
#6270=DIRECTION('center_axis',(0.,0.,1.));
#6271=DIRECTION('ref_axis',(1.,0.,0.));
#6272=DIRECTION('center_axis',(0.,0.,1.));
#6273=DIRECTION('ref_axis',(1.,0.,0.));
#6274=DIRECTION('center_axis',(0.,0.,1.));
#6275=DIRECTION('ref_axis',(1.,0.,0.));
#6276=DIRECTION('',(0.,0.,1.));
#6277=DIRECTION('center_axis',(0.,0.,1.));
#6278=DIRECTION('ref_axis',(1.,0.,0.));
#6279=DIRECTION('center_axis',(0.,0.,1.));
#6280=DIRECTION('ref_axis',(1.,0.,0.));
#6281=DIRECTION('center_axis',(0.,0.,1.));
#6282=DIRECTION('ref_axis',(1.,0.,0.));
#6283=DIRECTION('center_axis',(0.,0.,1.));
#6284=DIRECTION('ref_axis',(1.,0.,0.));
#6285=DIRECTION('',(0.,0.,1.));
#6286=DIRECTION('center_axis',(0.,0.,1.));
#6287=DIRECTION('ref_axis',(1.,0.,0.));
#6288=DIRECTION('center_axis',(0.,0.,1.));
#6289=DIRECTION('ref_axis',(1.,0.,0.));
#6290=DIRECTION('center_axis',(0.,0.,1.));
#6291=DIRECTION('ref_axis',(1.,0.,0.));
#6292=DIRECTION('center_axis',(0.,0.,1.));
#6293=DIRECTION('ref_axis',(1.,0.,0.));
#6294=DIRECTION('',(0.,0.,1.));
#6295=DIRECTION('center_axis',(0.,0.,1.));
#6296=DIRECTION('ref_axis',(1.,0.,0.));
#6297=DIRECTION('center_axis',(0.,0.,1.));
#6298=DIRECTION('ref_axis',(1.,0.,0.));
#6299=DIRECTION('center_axis',(0.,0.,1.));
#6300=DIRECTION('ref_axis',(1.,0.,0.));
#6301=DIRECTION('center_axis',(0.,0.,1.));
#6302=DIRECTION('ref_axis',(1.,0.,0.));
#6303=DIRECTION('',(0.,0.,1.));
#6304=DIRECTION('center_axis',(0.,0.,1.));
#6305=DIRECTION('ref_axis',(1.,0.,0.));
#6306=DIRECTION('center_axis',(0.,0.,1.));
#6307=DIRECTION('ref_axis',(1.,0.,0.));
#6308=DIRECTION('center_axis',(0.,0.,1.));
#6309=DIRECTION('ref_axis',(1.,0.,0.));
#6310=DIRECTION('center_axis',(0.,0.,1.));
#6311=DIRECTION('ref_axis',(1.,0.,0.));
#6312=DIRECTION('',(0.,0.,1.));
#6313=DIRECTION('center_axis',(0.,0.,-1.));
#6314=DIRECTION('ref_axis',(1.,0.,0.));
#6315=DIRECTION('center_axis',(0.,0.,1.));
#6316=DIRECTION('ref_axis',(1.,0.,0.));
#6317=DIRECTION('center_axis',(0.,0.,1.));
#6318=DIRECTION('ref_axis',(1.,0.,0.));
#6319=DIRECTION('center_axis',(0.,0.,1.));
#6320=DIRECTION('ref_axis',(1.,0.,0.));
#6321=DIRECTION('center_axis',(0.,0.,1.));
#6322=DIRECTION('ref_axis',(1.,0.,0.));
#6323=DIRECTION('',(0.,0.,1.));
#6324=DIRECTION('center_axis',(0.,1.,0.));
#6325=DIRECTION('ref_axis',(-1.,0.,0.));
#6326=DIRECTION('',(-1.,0.,0.));
#6327=DIRECTION('',(0.,0.,1.));
#6328=DIRECTION('',(-1.,0.,0.));
#6329=DIRECTION('',(0.,0.,1.));
#6330=DIRECTION('center_axis',(1.,0.,0.));
#6331=DIRECTION('ref_axis',(0.,1.,0.));
#6332=DIRECTION('',(0.,1.,0.));
#6333=DIRECTION('',(0.,1.,0.));
#6334=DIRECTION('',(0.,0.,1.));
#6335=DIRECTION('center_axis',(0.,-1.,0.));
#6336=DIRECTION('ref_axis',(1.,0.,0.));
#6337=DIRECTION('',(1.,0.,0.));
#6338=DIRECTION('',(1.,0.,0.));
#6339=DIRECTION('',(0.,0.,1.));
#6340=DIRECTION('center_axis',(-1.,0.,0.));
#6341=DIRECTION('ref_axis',(0.,-1.,0.));
#6342=DIRECTION('',(0.,-1.,0.));
#6343=DIRECTION('',(0.,-1.,0.));
#6344=DIRECTION('center_axis',(0.,0.,1.));
#6345=DIRECTION('ref_axis',(1.,0.,0.));
#6346=DIRECTION('center_axis',(0.,0.,1.));
#6347=DIRECTION('ref_axis',(1.,0.,0.));
#6348=DIRECTION('axis',(0.,0.,1.));
#6349=DIRECTION('refdir',(1.,0.,0.));
#6350=DIRECTION('center_axis',(0.,0.,1.));
#6351=DIRECTION('ref_axis',(1.,0.,0.));
#6352=DIRECTION('center_axis',(0.,0.,1.));
#6353=DIRECTION('ref_axis',(1.,0.,0.));
#6354=DIRECTION('',(0.,0.,1.));
#6355=DIRECTION('center_axis',(0.,0.,-1.));
#6356=DIRECTION('ref_axis',(1.,0.,0.));
#6357=DIRECTION('center_axis',(0.,0.,1.));
#6358=DIRECTION('ref_axis',(1.,0.,0.));
#6359=DIRECTION('center_axis',(0.,0.,1.));
#6360=DIRECTION('ref_axis',(1.,0.,0.));
#6361=DIRECTION('center_axis',(0.,0.,1.));
#6362=DIRECTION('ref_axis',(1.,0.,0.));
#6363=DIRECTION('center_axis',(0.,0.,1.));
#6364=DIRECTION('ref_axis',(1.,0.,0.));
#6365=DIRECTION('',(0.,0.,1.));
#6366=DIRECTION('center_axis',(0.,0.,-1.));
#6367=DIRECTION('ref_axis',(1.,0.,0.));
#6368=DIRECTION('center_axis',(0.,0.,1.));
#6369=DIRECTION('ref_axis',(1.,0.,0.));
#6370=DIRECTION('center_axis',(0.,0.,1.));
#6371=DIRECTION('ref_axis',(1.,0.,0.));
#6372=DIRECTION('center_axis',(0.,0.,1.));
#6373=DIRECTION('ref_axis',(1.,0.,0.));
#6374=DIRECTION('center_axis',(0.,0.,1.));
#6375=DIRECTION('ref_axis',(1.,0.,0.));
#6376=DIRECTION('',(0.,0.,1.));
#6377=DIRECTION('center_axis',(0.,0.,-1.));
#6378=DIRECTION('ref_axis',(1.,0.,0.));
#6379=DIRECTION('center_axis',(0.,0.,1.));
#6380=DIRECTION('ref_axis',(1.,0.,0.));
#6381=DIRECTION('center_axis',(0.,0.,1.));
#6382=DIRECTION('ref_axis',(1.,0.,0.));
#6383=DIRECTION('center_axis',(0.,0.,1.));
#6384=DIRECTION('ref_axis',(1.,0.,0.));
#6385=DIRECTION('center_axis',(0.,0.,1.));
#6386=DIRECTION('ref_axis',(1.,0.,0.));
#6387=DIRECTION('',(0.,0.,1.));
#6388=DIRECTION('center_axis',(0.,0.,-1.));
#6389=DIRECTION('ref_axis',(1.,0.,0.));
#6390=DIRECTION('center_axis',(0.,0.,1.));
#6391=DIRECTION('ref_axis',(1.,0.,0.));
#6392=DIRECTION('center_axis',(0.,0.,1.));
#6393=DIRECTION('ref_axis',(1.,0.,0.));
#6394=DIRECTION('center_axis',(0.,0.,1.));
#6395=DIRECTION('ref_axis',(1.,0.,0.));
#6396=DIRECTION('center_axis',(0.,0.,1.));
#6397=DIRECTION('ref_axis',(1.,0.,0.));
#6398=DIRECTION('',(0.,0.,1.));
#6399=DIRECTION('center_axis',(0.,0.,1.));
#6400=DIRECTION('ref_axis',(1.,0.,0.));
#6401=DIRECTION('center_axis',(0.,0.,1.));
#6402=DIRECTION('ref_axis',(1.,0.,0.));
#6403=DIRECTION('',(0.,0.,1.));
#6404=DIRECTION('center_axis',(0.,0.,1.));
#6405=DIRECTION('ref_axis',(1.,0.,0.));
#6406=DIRECTION('center_axis',(0.,0.,1.));
#6407=DIRECTION('ref_axis',(1.,0.,0.));
#6408=DIRECTION('',(0.,0.,1.));
#6409=DIRECTION('center_axis',(0.,0.,1.));
#6410=DIRECTION('ref_axis',(1.,0.,0.));
#6411=DIRECTION('center_axis',(0.,0.,1.));
#6412=DIRECTION('ref_axis',(1.,0.,0.));
#6413=DIRECTION('',(0.,0.,1.));
#6414=DIRECTION('center_axis',(0.,0.,1.));
#6415=DIRECTION('ref_axis',(1.,0.,0.));
#6416=DIRECTION('center_axis',(0.,0.,1.));
#6417=DIRECTION('ref_axis',(1.,0.,0.));
#6418=DIRECTION('',(0.,0.,-1.));
#6419=DIRECTION('center_axis',(0.,0.,1.));
#6420=DIRECTION('ref_axis',(1.,0.,0.));
#6421=DIRECTION('center_axis',(0.,0.,1.));
#6422=DIRECTION('ref_axis',(1.,0.,0.));
#6423=DIRECTION('center_axis',(0.,0.,-1.));
#6424=DIRECTION('ref_axis',(1.,0.,0.));
#6425=DIRECTION('center_axis',(0.,0.,1.));
#6426=DIRECTION('ref_axis',(1.,0.,0.));
#6427=DIRECTION('center_axis',(0.,0.,-1.));
#6428=DIRECTION('ref_axis',(1.,0.,0.));
#6429=DIRECTION('',(0.,0.,-1.));
#6430=DIRECTION('center_axis',(0.,0.,1.));
#6431=DIRECTION('ref_axis',(1.,0.,0.));
#6432=DIRECTION('center_axis',(0.,0.,1.));
#6433=DIRECTION('ref_axis',(1.,0.,0.));
#6434=DIRECTION('',(0.,0.,-1.));
#6435=DIRECTION('center_axis',(0.,0.,1.));
#6436=DIRECTION('ref_axis',(1.,0.,0.));
#6437=DIRECTION('center_axis',(0.,0.,1.));
#6438=DIRECTION('ref_axis',(1.,0.,0.));
#6439=DIRECTION('center_axis',(0.,0.,1.));
#6440=DIRECTION('ref_axis',(1.,0.,0.));
#6441=DIRECTION('axis',(0.,0.,1.));
#6442=DIRECTION('refdir',(1.,0.,0.));
#6443=DIRECTION('center_axis',(0.,0.,1.));
#6444=DIRECTION('ref_axis',(1.,0.,0.));
#6445=DIRECTION('center_axis',(0.,0.,-1.));
#6446=DIRECTION('ref_axis',(1.,0.,0.));
#6447=DIRECTION('',(0.,0.,-1.));
#6448=DIRECTION('center_axis',(0.,0.,-1.));
#6449=DIRECTION('ref_axis',(1.,0.,0.));
#6450=DIRECTION('center_axis',(0.,0.,1.));
#6451=DIRECTION('ref_axis',(1.,0.,0.));
#6452=DIRECTION('center_axis',(0.,0.,1.));
#6453=DIRECTION('ref_axis',(1.,0.,0.));
#6454=DIRECTION('',(0.,0.,-1.));
#6455=DIRECTION('center_axis',(0.,0.,1.));
#6456=DIRECTION('ref_axis',(1.,0.,0.));
#6457=DIRECTION('center_axis',(0.,0.,1.));
#6458=DIRECTION('ref_axis',(1.,0.,0.));
#6459=DIRECTION('center_axis',(0.,0.,1.));
#6460=DIRECTION('ref_axis',(1.,0.,0.));
#6461=DIRECTION('axis',(0.,0.,1.));
#6462=DIRECTION('refdir',(1.,0.,0.));
#6463=DIRECTION('center_axis',(-0.000134470403067858,0.996698884077706,
0.0811869225674069));
#6464=DIRECTION('ref_axis',(1.09533965337888E-5,-0.0811869218285139,0.996698893148795));
#6465=DIRECTION('center_axis',(0.000134470245157523,0.9966988840305,0.0811869231471977));
#6466=DIRECTION('ref_axis',(-0.0717698662269105,0.0809871795599261,-0.994127840395137));
#6467=DIRECTION('center_axis',(0.000134470245157523,0.9966988840305,0.0811869231471977));
#6468=DIRECTION('ref_axis',(-0.0717698662269105,0.0809871795599261,-0.994127840395137));
#6469=DIRECTION('center_axis',(-0.000134470403067858,0.996698884077706,
0.0811869225674069));
#6470=DIRECTION('ref_axis',(1.09533965337888E-5,-0.081186921828514,0.996698893148795));
#6471=DIRECTION('axis',(0.,0.,1.));
#6472=DIRECTION('refdir',(1.,0.,0.));
#6473=DIRECTION('center_axis',(0.,0.,1.));
#6474=DIRECTION('ref_axis',(1.,0.,0.));
#6475=DIRECTION('center_axis',(0.,0.,1.));
#6476=DIRECTION('ref_axis',(1.,0.,0.));
#6477=DIRECTION('',(0.,0.,1.));
#6478=DIRECTION('center_axis',(0.,0.,1.));
#6479=DIRECTION('ref_axis',(1.,0.,0.));
#6480=DIRECTION('center_axis',(0.,0.,1.));
#6481=DIRECTION('ref_axis',(1.,0.,0.));
#6482=DIRECTION('center_axis',(0.,0.,1.));
#6483=DIRECTION('ref_axis',(1.,0.,0.));
#6484=DIRECTION('',(0.,-1.,0.));
#6485=DIRECTION('',(1.,0.,0.));
#6486=DIRECTION('',(0.,-1.,0.));
#6487=DIRECTION('',(-1.,0.,0.));
#6488=DIRECTION('',(0.,1.,0.));
#6489=DIRECTION('',(1.,0.,0.));
#6490=DIRECTION('center_axis',(0.,1.,0.));
#6491=DIRECTION('ref_axis',(-1.,0.,0.));
#6492=DIRECTION('',(0.,0.,1.));
#6493=DIRECTION('',(-1.,0.,0.));
#6494=DIRECTION('',(0.,0.,1.));
#6495=DIRECTION('center_axis',(1.,0.,0.));
#6496=DIRECTION('ref_axis',(0.,1.,0.));
#6497=DIRECTION('',(0.,1.,0.));
#6498=DIRECTION('',(0.,0.,1.));
#6499=DIRECTION('center_axis',(0.,-1.,0.));
#6500=DIRECTION('ref_axis',(1.,0.,0.));
#6501=DIRECTION('',(0.,0.,1.));
#6502=DIRECTION('',(1.,0.,0.));
#6503=DIRECTION('',(0.,0.,1.));
#6504=DIRECTION('',(1.,0.,0.));
#6505=DIRECTION('center_axis',(-1.,0.,0.));
#6506=DIRECTION('ref_axis',(0.,-1.,0.));
#6507=DIRECTION('',(0.,0.,1.));
#6508=DIRECTION('',(0.,-1.,0.));
#6509=DIRECTION('',(0.,-1.,0.));
#6510=DIRECTION('center_axis',(0.,1.,0.));
#6511=DIRECTION('ref_axis',(-1.,0.,0.));
#6512=DIRECTION('',(0.,0.,1.));
#6513=DIRECTION('',(-1.,0.,0.));
#6514=DIRECTION('center_axis',(1.,0.,0.));
#6515=DIRECTION('ref_axis',(0.,1.,0.));
#6516=DIRECTION('',(0.,1.,0.));
#6517=DIRECTION('center_axis',(0.,0.,1.));
#6518=DIRECTION('ref_axis',(1.,0.,0.));
#6519=DIRECTION('center_axis',(0.,0.,1.));
#6520=DIRECTION('ref_axis',(1.,0.,0.));
#6521=DIRECTION('axis',(0.,0.,1.));
#6522=DIRECTION('refdir',(1.,0.,0.));
#6523=DIRECTION('center_axis',(0.,1.,0.));
#6524=DIRECTION('ref_axis',(1.,0.,0.));
#6525=DIRECTION('',(0.,1.,0.));
#6526=DIRECTION('center_axis',(0.,1.,0.));
#6527=DIRECTION('ref_axis',(1.,0.,0.));
#6528=DIRECTION('',(0.,1.,0.));
#6529=DIRECTION('center_axis',(0.,1.,0.));
#6530=DIRECTION('ref_axis',(1.,0.,0.));
#6531=DIRECTION('',(-1.,0.,0.));
#6532=DIRECTION('center_axis',(0.,1.,0.));
#6533=DIRECTION('ref_axis',(1.,0.,0.));
#6534=DIRECTION('center_axis',(0.,1.,0.));
#6535=DIRECTION('ref_axis',(1.,0.,0.));
#6536=DIRECTION('',(0.,-1.,0.));
#6537=DIRECTION('',(0.,1.,0.));
#6538=DIRECTION('center_axis',(0.,-1.,0.));
#6539=DIRECTION('ref_axis',(1.,0.,0.));
#6540=DIRECTION('',(0.,1.,0.));
#6541=DIRECTION('center_axis',(0.,0.,1.));
#6542=DIRECTION('ref_axis',(1.,0.,0.));
#6543=DIRECTION('center_axis',(0.,0.,1.));
#6544=DIRECTION('ref_axis',(1.,0.,0.));
#6545=DIRECTION('center_axis',(0.,0.,1.));
#6546=DIRECTION('ref_axis',(1.,0.,0.));
#6547=DIRECTION('center_axis',(0.,1.,0.));
#6548=DIRECTION('ref_axis',(1.,0.,0.));
#6549=DIRECTION('center_axis',(0.,1.,0.));
#6550=DIRECTION('ref_axis',(1.,0.,0.));
#6551=DIRECTION('',(0.,1.,0.));
#6552=DIRECTION('center_axis',(0.,-1.,0.));
#6553=DIRECTION('ref_axis',(1.,0.,0.));
#6554=DIRECTION('center_axis',(0.,1.,0.));
#6555=DIRECTION('ref_axis',(1.,0.,0.));
#6556=DIRECTION('center_axis',(0.,1.,0.));
#6557=DIRECTION('ref_axis',(1.,0.,0.));
#6558=DIRECTION('',(0.,1.,0.));
#6559=DIRECTION('center_axis',(0.,1.,0.));
#6560=DIRECTION('ref_axis',(1.,0.,0.));
#6561=DIRECTION('center_axis',(0.,1.,0.));
#6562=DIRECTION('ref_axis',(1.,0.,0.));
#6563=DIRECTION('center_axis',(0.,0.,1.));
#6564=DIRECTION('ref_axis',(1.,0.,0.));
#6565=DIRECTION('center_axis',(0.,0.,1.));
#6566=DIRECTION('ref_axis',(1.,0.,0.));
#6567=DIRECTION('center_axis',(0.,0.,1.));
#6568=DIRECTION('ref_axis',(1.,0.,0.));
#6569=DIRECTION('',(0.,0.,-1.));
#6570=DIRECTION('center_axis',(0.,0.,1.));
#6571=DIRECTION('ref_axis',(1.,0.,0.));
#6572=DIRECTION('center_axis',(0.,0.,1.));
#6573=DIRECTION('ref_axis',(1.,0.,0.));
#6574=DIRECTION('center_axis',(0.,0.,1.));
#6575=DIRECTION('ref_axis',(1.,0.,0.));
#6576=DIRECTION('',(0.,0.,1.));
#6577=DIRECTION('center_axis',(0.,0.,-1.));
#6578=DIRECTION('ref_axis',(1.,0.,0.));
#6579=DIRECTION('center_axis',(0.,0.,1.));
#6580=DIRECTION('ref_axis',(1.,0.,0.));
#6581=DIRECTION('center_axis',(0.,0.,1.));
#6582=DIRECTION('ref_axis',(1.,0.,0.));
#6583=DIRECTION('center_axis',(0.,0.,1.));
#6584=DIRECTION('ref_axis',(1.,0.,0.));
#6585=DIRECTION('',(0.,0.,1.));
#6586=DIRECTION('center_axis',(0.,0.,1.));
#6587=DIRECTION('ref_axis',(1.,0.,0.));
#6588=DIRECTION('center_axis',(0.,0.,1.));
#6589=DIRECTION('ref_axis',(1.,0.,0.));
#6590=DIRECTION('',(0.,0.,1.));
#6591=DIRECTION('center_axis',(0.,0.,-1.));
#6592=DIRECTION('ref_axis',(1.,0.,0.));
#6593=DIRECTION('center_axis',(0.,0.,1.));
#6594=DIRECTION('ref_axis',(1.,0.,0.));
#6595=DIRECTION('center_axis',(0.,0.,1.));
#6596=DIRECTION('ref_axis',(1.,0.,0.));
#6597=DIRECTION('',(0.,0.,1.));
#6598=DIRECTION('center_axis',(0.,0.,-1.));
#6599=DIRECTION('ref_axis',(1.,0.,0.));
#6600=DIRECTION('center_axis',(0.,0.,1.));
#6601=DIRECTION('ref_axis',(1.,0.,0.));
#6602=DIRECTION('center_axis',(0.,0.,1.));
#6603=DIRECTION('ref_axis',(1.,0.,0.));
#6604=DIRECTION('',(0.,0.,1.));
#6605=DIRECTION('center_axis',(0.,0.,-1.));
#6606=DIRECTION('ref_axis',(1.,0.,0.));
#6607=DIRECTION('center_axis',(0.,0.,1.));
#6608=DIRECTION('ref_axis',(1.,0.,0.));
#6609=DIRECTION('center_axis',(0.,0.,1.));
#6610=DIRECTION('ref_axis',(1.,0.,0.));
#6611=DIRECTION('',(0.,0.,1.));
#6612=DIRECTION('center_axis',(0.,0.,-1.));
#6613=DIRECTION('ref_axis',(1.,0.,0.));
#6614=DIRECTION('center_axis',(0.,0.,1.));
#6615=DIRECTION('ref_axis',(1.,0.,0.));
#6616=DIRECTION('center_axis',(0.,0.,1.));
#6617=DIRECTION('ref_axis',(1.,0.,0.));
#6618=DIRECTION('axis',(0.,0.,1.));
#6619=DIRECTION('refdir',(1.,0.,0.));
#6620=DIRECTION('center_axis',(0.,0.,1.));
#6621=DIRECTION('ref_axis',(1.,0.,0.));
#6622=DIRECTION('center_axis',(0.,0.,-1.));
#6623=DIRECTION('ref_axis',(1.,0.,0.));
#6624=DIRECTION('',(0.,0.,-1.));
#6625=DIRECTION('center_axis',(0.,0.,-1.));
#6626=DIRECTION('ref_axis',(1.,0.,0.));
#6627=DIRECTION('center_axis',(0.,0.,1.));
#6628=DIRECTION('ref_axis',(1.,0.,0.));
#6629=DIRECTION('center_axis',(0.,0.,1.));
#6630=DIRECTION('ref_axis',(1.,0.,0.));
#6631=DIRECTION('',(0.,0.,-1.));
#6632=DIRECTION('center_axis',(0.,0.,1.));
#6633=DIRECTION('ref_axis',(1.,0.,0.));
#6634=DIRECTION('center_axis',(0.,0.,1.));
#6635=DIRECTION('ref_axis',(1.,0.,0.));
#6636=DIRECTION('center_axis',(0.,0.,1.));
#6637=DIRECTION('ref_axis',(1.,0.,0.));
#6638=DIRECTION('axis',(0.,0.,1.));
#6639=DIRECTION('refdir',(1.,0.,0.));
#6640=DIRECTION('center_axis',(0.,0.,1.));
#6641=DIRECTION('ref_axis',(1.,0.,0.));
#6642=DIRECTION('',(-1.,0.,0.));
#6643=DIRECTION('center_axis',(0.,0.,1.));
#6644=DIRECTION('ref_axis',(1.,0.,0.));
#6645=DIRECTION('center_axis',(0.,0.,1.));
#6646=DIRECTION('ref_axis',(1.,0.,0.));
#6647=DIRECTION('center_axis',(0.,0.,1.));
#6648=DIRECTION('ref_axis',(1.,0.,0.));
#6649=DIRECTION('',(0.,0.,1.));
#6650=DIRECTION('',(0.,0.,-1.));
#6651=DIRECTION('',(0.,0.,1.));
#6652=DIRECTION('center_axis',(0.,1.,0.));
#6653=DIRECTION('ref_axis',(1.,0.,0.));
#6654=DIRECTION('center_axis',(0.,1.,0.));
#6655=DIRECTION('ref_axis',(1.,0.,0.));
#6656=DIRECTION('center_axis',(0.,1.,0.));
#6657=DIRECTION('ref_axis',(1.,0.,0.));
#6658=DIRECTION('center_axis',(0.,1.,0.));
#6659=DIRECTION('ref_axis',(1.,0.,0.));
#6660=DIRECTION('',(0.,1.,0.));
#6661=DIRECTION('center_axis',(0.,-1.,0.));
#6662=DIRECTION('ref_axis',(1.,0.,0.));
#6663=DIRECTION('center_axis',(0.,1.,0.));
#6664=DIRECTION('ref_axis',(1.,0.,0.));
#6665=DIRECTION('center_axis',(0.,1.,0.));
#6666=DIRECTION('ref_axis',(1.,0.,0.));
#6667=DIRECTION('',(0.,1.,0.));
#6668=DIRECTION('center_axis',(0.,-1.,0.));
#6669=DIRECTION('ref_axis',(1.,0.,0.));
#6670=DIRECTION('center_axis',(0.,1.,0.));
#6671=DIRECTION('ref_axis',(1.,0.,0.));
#6672=DIRECTION('center_axis',(0.,1.,0.));
#6673=DIRECTION('ref_axis',(1.,0.,0.));
#6674=DIRECTION('center_axis',(0.,1.,0.));
#6675=DIRECTION('ref_axis',(1.,0.,0.));
#6676=DIRECTION('',(0.,1.,0.));
#6677=DIRECTION('center_axis',(0.,1.,0.));
#6678=DIRECTION('ref_axis',(1.,0.,0.));
#6679=DIRECTION('center_axis',(0.,0.,1.));
#6680=DIRECTION('ref_axis',(1.,0.,0.));
#6681=DIRECTION('center_axis',(0.,0.,1.));
#6682=DIRECTION('ref_axis',(1.,0.,0.));
#6683=DIRECTION('',(0.,0.,1.));
#6684=DIRECTION('center_axis',(0.,0.,1.));
#6685=DIRECTION('ref_axis',(1.,0.,0.));
#6686=DIRECTION('center_axis',(0.,0.,1.));
#6687=DIRECTION('ref_axis',(1.,0.,0.));
#6688=DIRECTION('center_axis',(0.,0.,-1.));
#6689=DIRECTION('ref_axis',(1.,0.,0.));
#6690=DIRECTION('center_axis',(0.,0.,1.));
#6691=DIRECTION('ref_axis',(1.,0.,0.));
#6692=DIRECTION('center_axis',(0.,0.,1.));
#6693=DIRECTION('ref_axis',(1.,0.,0.));
#6694=DIRECTION('center_axis',(0.,0.,1.));
#6695=DIRECTION('ref_axis',(1.,0.,0.));
#6696=DIRECTION('center_axis',(0.,0.,1.));
#6697=DIRECTION('ref_axis',(1.,0.,0.));
#6698=DIRECTION('',(0.,0.,1.));
#6699=DIRECTION('center_axis',(0.,0.,1.));
#6700=DIRECTION('ref_axis',(1.,0.,0.));
#6701=DIRECTION('',(0.,0.,1.));
#6702=DIRECTION('center_axis',(0.,0.,-1.));
#6703=DIRECTION('ref_axis',(1.,0.,0.));
#6704=DIRECTION('center_axis',(0.,0.,1.));
#6705=DIRECTION('ref_axis',(1.,0.,0.));
#6706=DIRECTION('center_axis',(0.,0.,1.));
#6707=DIRECTION('ref_axis',(1.,0.,0.));
#6708=DIRECTION('',(0.,0.,1.));
#6709=DIRECTION('center_axis',(0.,0.,1.));
#6710=DIRECTION('ref_axis',(1.,0.,0.));
#6711=DIRECTION('center_axis',(0.,0.,1.));
#6712=DIRECTION('ref_axis',(1.,0.,0.));
#6713=DIRECTION('center_axis',(0.,0.,-1.));
#6714=DIRECTION('ref_axis',(1.,0.,0.));
#6715=DIRECTION('center_axis',(0.,0.,1.));
#6716=DIRECTION('ref_axis',(1.,0.,0.));
#6717=DIRECTION('',(0.,0.,1.));
#6718=DIRECTION('center_axis',(0.,0.,1.));
#6719=DIRECTION('ref_axis',(1.,0.,0.));
#6720=DIRECTION('center_axis',(0.,0.,1.));
#6721=DIRECTION('ref_axis',(1.,0.,0.));
#6722=DIRECTION('center_axis',(0.,0.,1.));
#6723=DIRECTION('ref_axis',(1.,0.,0.));
#6724=DIRECTION('center_axis',(0.,0.,1.));
#6725=DIRECTION('ref_axis',(1.,0.,0.));
#6726=DIRECTION('',(0.,0.,1.));
#6727=DIRECTION('center_axis',(0.,0.,-1.));
#6728=DIRECTION('ref_axis',(1.,0.,0.));
#6729=DIRECTION('center_axis',(0.,0.,1.));
#6730=DIRECTION('ref_axis',(1.,0.,0.));
#6731=DIRECTION('center_axis',(0.,0.,1.));
#6732=DIRECTION('ref_axis',(1.,0.,0.));
#6733=DIRECTION('',(0.,0.,1.));
#6734=DIRECTION('center_axis',(0.,0.,-1.));
#6735=DIRECTION('ref_axis',(1.,0.,0.));
#6736=DIRECTION('center_axis',(0.,0.,1.));
#6737=DIRECTION('ref_axis',(1.,0.,0.));
#6738=DIRECTION('center_axis',(0.,0.,1.));
#6739=DIRECTION('ref_axis',(1.,0.,0.));
#6740=DIRECTION('',(0.,0.,1.));
#6741=DIRECTION('center_axis',(0.,0.,-1.));
#6742=DIRECTION('ref_axis',(1.,0.,0.));
#6743=DIRECTION('center_axis',(0.,0.,1.));
#6744=DIRECTION('ref_axis',(1.,0.,0.));
#6745=DIRECTION('center_axis',(0.,0.,1.));
#6746=DIRECTION('ref_axis',(1.,0.,0.));
#6747=DIRECTION('',(0.,0.,1.));
#6748=DIRECTION('center_axis',(0.,0.,-1.));
#6749=DIRECTION('ref_axis',(1.,0.,0.));
#6750=DIRECTION('center_axis',(0.,0.,1.));
#6751=DIRECTION('ref_axis',(1.,0.,0.));
#6752=DIRECTION('center_axis',(0.,0.,1.));
#6753=DIRECTION('ref_axis',(1.,0.,0.));
#6754=DIRECTION('',(0.,0.,-1.));
#6755=DIRECTION('center_axis',(0.,0.,1.));
#6756=DIRECTION('ref_axis',(1.,0.,0.));
#6757=DIRECTION('center_axis',(0.,0.,1.));
#6758=DIRECTION('ref_axis',(1.,0.,0.));
#6759=DIRECTION('center_axis',(0.,0.,1.));
#6760=DIRECTION('ref_axis',(1.,0.,0.));
#6761=DIRECTION('axis',(0.,0.,1.));
#6762=DIRECTION('refdir',(1.,0.,0.));
#6763=DIRECTION('center_axis',(0.,0.,1.));
#6764=DIRECTION('ref_axis',(1.,0.,0.));
#6765=DIRECTION('center_axis',(0.,0.,-1.));
#6766=DIRECTION('ref_axis',(1.,0.,0.));
#6767=DIRECTION('',(0.,0.,-1.));
#6768=DIRECTION('center_axis',(0.,0.,-1.));
#6769=DIRECTION('ref_axis',(1.,0.,0.));
#6770=DIRECTION('center_axis',(0.,0.,1.));
#6771=DIRECTION('ref_axis',(1.,0.,0.));
#6772=DIRECTION('center_axis',(0.,0.,1.));
#6773=DIRECTION('ref_axis',(1.,0.,0.));
#6774=DIRECTION('',(0.,0.,-1.));
#6775=DIRECTION('center_axis',(0.,0.,1.));
#6776=DIRECTION('ref_axis',(1.,0.,0.));
#6777=DIRECTION('center_axis',(0.,0.,1.));
#6778=DIRECTION('ref_axis',(1.,0.,0.));
#6779=DIRECTION('center_axis',(0.,0.,1.));
#6780=DIRECTION('ref_axis',(1.,0.,0.));
#6781=DIRECTION('axis',(0.,0.,1.));
#6782=DIRECTION('refdir',(1.,0.,0.));
#6783=DIRECTION('center_axis',(0.,0.,1.));
#6784=DIRECTION('ref_axis',(1.,0.,0.));
#6785=DIRECTION('center_axis',(0.,0.,-1.));
#6786=DIRECTION('ref_axis',(1.,0.,0.));
#6787=DIRECTION('',(0.,0.,-1.));
#6788=DIRECTION('center_axis',(0.,0.,-1.));
#6789=DIRECTION('ref_axis',(1.,0.,0.));
#6790=DIRECTION('center_axis',(0.,0.,1.));
#6791=DIRECTION('ref_axis',(1.,0.,0.));
#6792=DIRECTION('center_axis',(0.,0.,1.));
#6793=DIRECTION('ref_axis',(1.,0.,0.));
#6794=DIRECTION('',(0.,0.,-1.));
#6795=DIRECTION('center_axis',(0.,0.,1.));
#6796=DIRECTION('ref_axis',(1.,0.,0.));
#6797=DIRECTION('center_axis',(0.,0.,1.));
#6798=DIRECTION('ref_axis',(1.,0.,0.));
#6799=DIRECTION('center_axis',(0.,0.,1.));
#6800=DIRECTION('ref_axis',(1.,0.,0.));
#6801=DIRECTION('axis',(0.,0.,1.));
#6802=DIRECTION('refdir',(1.,0.,0.));
#6803=DIRECTION('center_axis',(0.,0.,1.));
#6804=DIRECTION('ref_axis',(1.,0.,0.));
#6805=DIRECTION('center_axis',(0.,0.,-1.));
#6806=DIRECTION('ref_axis',(1.,0.,0.));
#6807=DIRECTION('',(0.,0.,-1.));
#6808=DIRECTION('center_axis',(0.,0.,-1.));
#6809=DIRECTION('ref_axis',(1.,0.,0.));
#6810=DIRECTION('center_axis',(0.,0.,1.));
#6811=DIRECTION('ref_axis',(1.,0.,0.));
#6812=DIRECTION('center_axis',(0.,0.,1.));
#6813=DIRECTION('ref_axis',(1.,0.,0.));
#6814=DIRECTION('',(0.,0.,-1.));
#6815=DIRECTION('center_axis',(0.,0.,1.));
#6816=DIRECTION('ref_axis',(1.,0.,0.));
#6817=DIRECTION('center_axis',(0.,0.,1.));
#6818=DIRECTION('ref_axis',(1.,0.,0.));
#6819=DIRECTION('center_axis',(0.,0.,1.));
#6820=DIRECTION('ref_axis',(1.,0.,0.));
#6821=DIRECTION('axis',(0.,0.,1.));
#6822=DIRECTION('refdir',(1.,0.,0.));
#6823=DIRECTION('center_axis',(0.,0.,1.));
#6824=DIRECTION('ref_axis',(1.,0.,0.));
#6825=DIRECTION('center_axis',(0.,0.,1.));
#6826=DIRECTION('ref_axis',(1.,0.,0.));
#6827=DIRECTION('',(0.,0.,-1.));
#6828=DIRECTION('center_axis',(0.,0.,1.));
#6829=DIRECTION('ref_axis',(1.,0.,0.));
#6830=DIRECTION('center_axis',(0.,0.,1.));
#6831=DIRECTION('ref_axis',(1.,0.,0.));
#6832=DIRECTION('center_axis',(0.,0.,1.));
#6833=DIRECTION('ref_axis',(1.,0.,0.));
#6834=DIRECTION('axis',(0.,0.,1.));
#6835=DIRECTION('refdir',(1.,0.,0.));
#6836=DIRECTION('center_axis',(0.,0.,1.));
#6837=DIRECTION('ref_axis',(1.,0.,0.));
#6838=DIRECTION('center_axis',(0.,0.,1.));
#6839=DIRECTION('ref_axis',(1.,0.,0.));
#6840=DIRECTION('',(0.,0.,-1.));
#6841=DIRECTION('center_axis',(0.,0.,1.));
#6842=DIRECTION('ref_axis',(1.,0.,0.));
#6843=DIRECTION('center_axis',(0.,0.,1.));
#6844=DIRECTION('ref_axis',(1.,0.,0.));
#6845=DIRECTION('center_axis',(0.,0.,1.));
#6846=DIRECTION('ref_axis',(1.,0.,0.));
#6847=DIRECTION('axis',(0.,0.,1.));
#6848=DIRECTION('refdir',(1.,0.,0.));
#6849=DIRECTION('center_axis',(0.,0.,1.));
#6850=DIRECTION('ref_axis',(1.,0.,0.));
#6851=DIRECTION('center_axis',(0.,0.,1.));
#6852=DIRECTION('ref_axis',(1.,0.,0.));
#6853=DIRECTION('',(0.,0.,-1.));
#6854=DIRECTION('center_axis',(0.,0.,1.));
#6855=DIRECTION('ref_axis',(1.,0.,0.));
#6856=DIRECTION('center_axis',(0.,0.,1.));
#6857=DIRECTION('ref_axis',(1.,0.,0.));
#6858=DIRECTION('center_axis',(0.,0.,1.));
#6859=DIRECTION('ref_axis',(1.,0.,0.));
#6860=DIRECTION('axis',(0.,0.,1.));
#6861=DIRECTION('refdir',(1.,0.,0.));
#6862=DIRECTION('center_axis',(0.,0.,1.));
#6863=DIRECTION('ref_axis',(1.,0.,0.));
#6864=DIRECTION('center_axis',(0.,0.,1.));
#6865=DIRECTION('ref_axis',(1.,0.,0.));
#6866=DIRECTION('',(0.,0.,-1.));
#6867=DIRECTION('center_axis',(0.,0.,1.));
#6868=DIRECTION('ref_axis',(1.,0.,0.));
#6869=DIRECTION('center_axis',(0.,0.,1.));
#6870=DIRECTION('ref_axis',(1.,0.,0.));
#6871=DIRECTION('center_axis',(0.,0.,1.));
#6872=DIRECTION('ref_axis',(1.,0.,0.));
#6873=DIRECTION('axis',(0.,0.,1.));
#6874=DIRECTION('refdir',(1.,0.,0.));
#6875=DIRECTION('axis',(0.,0.,1.));
#6876=DIRECTION('refdir',(1.,0.,0.));
#6877=DIRECTION('center_axis',(0.,1.,0.));
#6878=DIRECTION('ref_axis',(0.,0.,1.));
#6879=DIRECTION('center_axis',(0.,-1.,0.));
#6880=DIRECTION('ref_axis',(1.,0.,0.));
#6881=DIRECTION('',(-1.,0.,0.));
#6882=DIRECTION('',(0.,0.,-1.));
#6883=DIRECTION('',(1.,0.,0.));
#6884=DIRECTION('center_axis',(0.,0.,1.));
#6885=DIRECTION('ref_axis',(1.,0.,0.));
#6886=DIRECTION('',(0.,-1.,0.));
#6887=DIRECTION('',(0.,1.,0.));
#6888=DIRECTION('',(-1.,0.,0.));
#6889=DIRECTION('center_axis',(0.,-1.,0.));
#6890=DIRECTION('ref_axis',(0.,0.,-1.));
#6891=DIRECTION('center_axis',(0.,1.,0.));
#6892=DIRECTION('ref_axis',(1.,0.,0.));
#6893=DIRECTION('',(0.,0.,1.));
#6894=DIRECTION('',(1.,0.,0.));
#6895=DIRECTION('center_axis',(0.,0.,-1.));
#6896=DIRECTION('ref_axis',(-1.,0.,0.));
#6897=DIRECTION('',(0.,1.,0.));
#6898=DIRECTION('',(0.,1.,0.));
#6899=DIRECTION('center_axis',(1.,0.,0.));
#6900=DIRECTION('ref_axis',(0.,0.,-1.));
#6901=DIRECTION('center_axis',(0.,1.,0.));
#6902=DIRECTION('ref_axis',(0.,0.,1.));
#6903=DIRECTION('center_axis',(0.,-1.,0.));
#6904=DIRECTION('ref_axis',(1.,0.,0.));
#6905=DIRECTION('center_axis',(0.,-1.,0.));
#6906=DIRECTION('ref_axis',(1.,0.,0.));
#6907=DIRECTION('center_axis',(0.,-1.,0.));
#6908=DIRECTION('ref_axis',(1.,0.,0.));
#6909=DIRECTION('center_axis',(0.,-1.,0.));
#6910=DIRECTION('ref_axis',(1.,0.,0.));
#6911=DIRECTION('',(0.,1.,0.));
#6912=DIRECTION('center_axis',(0.,-1.,0.));
#6913=DIRECTION('ref_axis',(0.,0.,-1.));
#6914=DIRECTION('center_axis',(0.,-1.,0.));
#6915=DIRECTION('ref_axis',(1.,0.,0.));
#6916=DIRECTION('center_axis',(0.,-1.,0.));
#6917=DIRECTION('ref_axis',(1.,0.,0.));
#6918=DIRECTION('center_axis',(0.,-1.,0.));
#6919=DIRECTION('ref_axis',(1.,0.,0.));
#6920=DIRECTION('',(0.,1.,0.));
#6921=DIRECTION('center_axis',(0.,1.,0.));
#6922=DIRECTION('ref_axis',(0.,0.,1.));
#6923=DIRECTION('center_axis',(0.,-1.,0.));
#6924=DIRECTION('ref_axis',(1.,0.,0.));
#6925=DIRECTION('center_axis',(0.,-1.,0.));
#6926=DIRECTION('ref_axis',(1.,0.,0.));
#6927=DIRECTION('center_axis',(0.,-1.,0.));
#6928=DIRECTION('ref_axis',(1.,0.,0.));
#6929=DIRECTION('',(0.,1.,0.));
#6930=DIRECTION('center_axis',(0.,-1.,0.));
#6931=DIRECTION('ref_axis',(0.,0.,-1.));
#6932=DIRECTION('center_axis',(0.,-1.,0.));
#6933=DIRECTION('ref_axis',(1.,0.,0.));
#6934=DIRECTION('center_axis',(0.,-1.,0.));
#6935=DIRECTION('ref_axis',(1.,0.,0.));
#6936=DIRECTION('center_axis',(0.,-1.,0.));
#6937=DIRECTION('ref_axis',(1.,0.,0.));
#6938=DIRECTION('',(0.,1.,0.));
#6939=DIRECTION('center_axis',(0.,1.,0.));
#6940=DIRECTION('ref_axis',(0.,0.,1.));
#6941=DIRECTION('center_axis',(0.,-1.,0.));
#6942=DIRECTION('ref_axis',(1.,0.,0.));
#6943=DIRECTION('center_axis',(0.,-1.,0.));
#6944=DIRECTION('ref_axis',(1.,0.,0.));
#6945=DIRECTION('center_axis',(0.,-1.,0.));
#6946=DIRECTION('ref_axis',(1.,0.,0.));
#6947=DIRECTION('',(0.,1.,0.));
#6948=DIRECTION('center_axis',(0.,-1.,0.));
#6949=DIRECTION('ref_axis',(0.,0.,-1.));
#6950=DIRECTION('center_axis',(0.,-1.,0.));
#6951=DIRECTION('ref_axis',(1.,0.,0.));
#6952=DIRECTION('center_axis',(0.,-1.,0.));
#6953=DIRECTION('ref_axis',(1.,0.,0.));
#6954=DIRECTION('',(0.,1.,0.));
#6955=DIRECTION('axis',(0.,0.,1.));
#6956=DIRECTION('refdir',(1.,0.,0.));
#6957=DIRECTION('center_axis',(0.,1.,0.));
#6958=DIRECTION('ref_axis',(0.,0.,1.));
#6959=DIRECTION('center_axis',(0.,1.,0.));
#6960=DIRECTION('ref_axis',(1.,0.,0.));
#6961=DIRECTION('',(1.,0.,0.));
#6962=DIRECTION('center_axis',(0.,-1.,0.));
#6963=DIRECTION('ref_axis',(1.,0.,0.));
#6964=DIRECTION('',(-1.,0.,0.));
#6965=DIRECTION('center_axis',(0.,0.,-1.));
#6966=DIRECTION('ref_axis',(-1.,0.,0.));
#6967=DIRECTION('',(0.,-1.,0.));
#6968=DIRECTION('',(0.,1.,0.));
#6969=DIRECTION('',(1.,0.,0.));
#6970=DIRECTION('center_axis',(0.,-1.,0.));
#6971=DIRECTION('ref_axis',(0.,0.,-1.));
#6972=DIRECTION('center_axis',(0.,-1.,0.));
#6973=DIRECTION('ref_axis',(1.,0.,0.));
#6974=DIRECTION('center_axis',(0.,1.,0.));
#6975=DIRECTION('ref_axis',(1.,0.,0.));
#6976=DIRECTION('',(-1.,0.,0.));
#6977=DIRECTION('center_axis',(0.,0.,1.));
#6978=DIRECTION('ref_axis',(1.,0.,0.));
#6979=DIRECTION('',(0.,1.,0.));
#6980=DIRECTION('',(0.,-1.,0.));
#6981=DIRECTION('center_axis',(0.,1.,0.));
#6982=DIRECTION('ref_axis',(0.,0.,1.));
#6983=DIRECTION('center_axis',(0.,-1.,0.));
#6984=DIRECTION('ref_axis',(1.,0.,0.));
#6985=DIRECTION('center_axis',(0.,-1.,0.));
#6986=DIRECTION('ref_axis',(1.,0.,0.));
#6987=DIRECTION('center_axis',(0.,-1.,0.));
#6988=DIRECTION('ref_axis',(1.,0.,0.));
#6989=DIRECTION('center_axis',(0.,-1.,0.));
#6990=DIRECTION('ref_axis',(1.,0.,0.));
#6991=DIRECTION('',(0.,1.,0.));
#6992=DIRECTION('center_axis',(0.,-1.,0.));
#6993=DIRECTION('ref_axis',(0.,0.,-1.));
#6994=DIRECTION('center_axis',(0.,-1.,0.));
#6995=DIRECTION('ref_axis',(1.,0.,0.));
#6996=DIRECTION('center_axis',(0.,-1.,0.));
#6997=DIRECTION('ref_axis',(1.,0.,0.));
#6998=DIRECTION('',(0.,1.,0.));
#6999=DIRECTION('',(0.,0.,1.));
#7000=DIRECTION('',(1.,0.,0.));
#7001=DIRECTION('',(0.,0.,1.));
#7002=DIRECTION('',(1.,0.,0.));
#7003=DIRECTION('axis',(0.,0.,1.));
#7004=DIRECTION('refdir',(1.,0.,0.));
#7005=DIRECTION('center_axis',(0.,1.,0.));
#7006=DIRECTION('ref_axis',(0.,0.,1.));
#7007=DIRECTION('center_axis',(0.,-1.,0.));
#7008=DIRECTION('ref_axis',(1.,0.,0.));
#7009=DIRECTION('center_axis',(0.,-1.,0.));
#7010=DIRECTION('ref_axis',(1.,0.,0.));
#7011=DIRECTION('center_axis',(0.,-1.,0.));
#7012=DIRECTION('ref_axis',(1.,0.,0.));
#7013=DIRECTION('',(0.707106781186548,0.707106781186547,8.65956056235493E-17));
#7014=DIRECTION('center_axis',(0.,-1.,0.));
#7015=DIRECTION('ref_axis',(1.,0.,0.));
#7016=DIRECTION('center_axis',(0.,-1.,0.));
#7017=DIRECTION('ref_axis',(1.,0.,0.));
#7018=DIRECTION('',(0.,1.,0.));
#7019=DIRECTION('center_axis',(0.,1.,0.));
#7020=DIRECTION('ref_axis',(1.,0.,0.));
#7021=DIRECTION('center_axis',(0.,-1.,0.));
#7022=DIRECTION('ref_axis',(1.,0.,0.));
#7023=DIRECTION('',(-0.707106781186547,0.707106781186548,-8.65956056235493E-17));
#7024=DIRECTION('center_axis',(0.,-1.,0.));
#7025=DIRECTION('ref_axis',(0.,0.,-1.));
#7026=DIRECTION('center_axis',(0.,-1.,0.));
#7027=DIRECTION('ref_axis',(1.,0.,0.));
#7028=DIRECTION('center_axis',(0.,1.,0.));
#7029=DIRECTION('ref_axis',(1.,0.,0.));
#7030=DIRECTION('center_axis',(0.,1.,0.));
#7031=DIRECTION('ref_axis',(1.,0.,0.));
#7032=DIRECTION('',(-0.447213595499958,0.894427190999916,-5.47678698264203E-17));
#7033=DIRECTION('center_axis',(0.,-1.,0.));
#7034=DIRECTION('ref_axis',(1.,0.,0.));
#7035=DIRECTION('center_axis',(0.,1.,0.));
#7036=DIRECTION('ref_axis',(1.,0.,0.));
#7037=DIRECTION('',(0.,1.,0.));
#7038=DIRECTION('center_axis',(0.,1.,0.));
#7039=DIRECTION('ref_axis',(1.,0.,0.));
#7040=DIRECTION('center_axis',(0.,-1.,0.));
#7041=DIRECTION('ref_axis',(1.,0.,0.));
#7042=DIRECTION('',(-0.707106781186547,0.707106781186548,-8.65956056235493E-17));
#7043=DIRECTION('center_axis',(0.,-1.,0.));
#7044=DIRECTION('ref_axis',(0.,0.,-1.));
#7045=DIRECTION('center_axis',(0.866025403784439,0.,-0.5));
#7046=DIRECTION('ref_axis',(0.5,0.,0.866025403784439));
#7047=DIRECTION('',(-0.5,0.,-0.866025403784439));
#7048=DIRECTION('',(0.,-1.,0.));
#7049=DIRECTION('',(0.5,0.,0.866025403784439));
#7050=DIRECTION('',(0.,-1.,0.));
#7051=DIRECTION('center_axis',(1.20185167898973E-16,0.,-1.));
#7052=DIRECTION('ref_axis',(1.,0.,1.20185167898973E-16));
#7053=DIRECTION('',(-1.,0.,-1.20185167898973E-16));
#7054=DIRECTION('',(0.,-1.,0.));
#7055=DIRECTION('',(1.,0.,1.20185167898973E-16));
#7056=DIRECTION('center_axis',(-0.866025403784439,0.,-0.5));
#7057=DIRECTION('ref_axis',(0.5,0.,-0.866025403784439));
#7058=DIRECTION('',(-0.5,0.,0.866025403784439));
#7059=DIRECTION('',(0.,-1.,0.));
#7060=DIRECTION('',(0.5,0.,-0.866025403784439));
#7061=DIRECTION('center_axis',(-0.866025403784439,0.,0.5));
#7062=DIRECTION('ref_axis',(-0.5,0.,-0.866025403784439));
#7063=DIRECTION('',(0.5,0.,0.866025403784439));
#7064=DIRECTION('',(0.,-1.,0.));
#7065=DIRECTION('',(-0.5,0.,-0.866025403784439));
#7066=DIRECTION('center_axis',(-2.40370335797945E-16,0.,1.));
#7067=DIRECTION('ref_axis',(-1.,0.,-2.40370335797945E-16));
#7068=DIRECTION('',(1.,0.,2.40370335797945E-16));
#7069=DIRECTION('',(0.,-1.,0.));
#7070=DIRECTION('',(-1.,0.,-2.40370335797945E-16));
#7071=DIRECTION('center_axis',(0.866025403784439,0.,0.5));
#7072=DIRECTION('ref_axis',(-0.5,0.,0.866025403784439));
#7073=DIRECTION('',(0.5,0.,-0.866025403784439));
#7074=DIRECTION('',(-0.5,0.,0.866025403784439));
#7075=DIRECTION('center_axis',(0.,1.,0.));
#7076=DIRECTION('ref_axis',(1.,0.,0.));
#7077=DIRECTION('center_axis',(0.,-1.,0.));
#7078=DIRECTION('ref_axis',(0.,0.,-1.));
#7079=DIRECTION('axis',(0.,0.,1.));
#7080=DIRECTION('refdir',(1.,0.,0.));
#7081=DIRECTION('axis',(0.,0.,1.));
#7082=DIRECTION('refdir',(1.,0.,0.));
#7083=DIRECTION('center_axis',(0.,1.,0.));
#7084=DIRECTION('ref_axis',(1.,0.,0.));
#7085=DIRECTION('center_axis',(0.,1.,0.));
#7086=DIRECTION('ref_axis',(1.,0.,0.));
#7087=DIRECTION('',(0.,1.,0.));
#7088=DIRECTION('center_axis',(0.,-1.,0.));
#7089=DIRECTION('ref_axis',(1.,0.,0.));
#7090=DIRECTION('center_axis',(0.,1.,0.));
#7091=DIRECTION('ref_axis',(1.,0.,0.));
#7092=DIRECTION('center_axis',(0.,1.,0.));
#7093=DIRECTION('ref_axis',(1.,0.,0.));
#7094=DIRECTION('center_axis',(0.,1.,0.));
#7095=DIRECTION('ref_axis',(1.,0.,0.));
#7096=DIRECTION('',(0.5,0.,-0.866025403784439));
#7097=DIRECTION('',(-0.5,0.,-0.866025403784439));
#7098=DIRECTION('',(-1.,0.,-1.60246890531964E-16));
#7099=DIRECTION('',(-0.5,0.,0.866025403784439));
#7100=DIRECTION('',(0.5,0.,0.866025403784439));
#7101=DIRECTION('',(1.,0.,1.60246890531964E-16));
#7102=DIRECTION('center_axis',(0.,-1.,0.));
#7103=DIRECTION('ref_axis',(1.,0.,0.));
#7104=DIRECTION('center_axis',(0.,1.,0.));
#7105=DIRECTION('ref_axis',(1.,0.,0.));
#7106=DIRECTION('',(0.5,0.,-0.866025403784439));
#7107=DIRECTION('',(1.,0.,1.60246890531964E-16));
#7108=DIRECTION('',(0.5,0.,0.866025403784439));
#7109=DIRECTION('',(-0.5,0.,0.866025403784439));
#7110=DIRECTION('',(-1.,0.,-1.60246890531964E-16));
#7111=DIRECTION('',(-0.5,0.,-0.866025403784439));
#7112=DIRECTION('center_axis',(0.,-1.,0.));
#7113=DIRECTION('ref_axis',(1.,0.,0.));
#7114=DIRECTION('center_axis',(-1.60246890531964E-16,0.,1.));
#7115=DIRECTION('ref_axis',(1.,0.,1.60246890531964E-16));
#7116=DIRECTION('',(0.,1.,0.));
#7117=DIRECTION('',(0.,1.,0.));
#7118=DIRECTION('center_axis',(-0.866025403784439,0.,0.5));
#7119=DIRECTION('ref_axis',(0.5,0.,0.866025403784439));
#7120=DIRECTION('',(0.,1.,0.));
#7121=DIRECTION('center_axis',(-0.866025403784439,0.,-0.5));
#7122=DIRECTION('ref_axis',(-0.5,0.,0.866025403784439));
#7123=DIRECTION('',(0.,1.,0.));
#7124=DIRECTION('center_axis',(1.60246890531964E-16,0.,-1.));
#7125=DIRECTION('ref_axis',(-1.,0.,-1.60246890531964E-16));
#7126=DIRECTION('',(0.,1.,0.));
#7127=DIRECTION('center_axis',(0.866025403784439,0.,-0.5));
#7128=DIRECTION('ref_axis',(-0.5,0.,-0.866025403784439));
#7129=DIRECTION('',(0.,1.,0.));
#7130=DIRECTION('center_axis',(0.866025403784439,0.,0.5));
#7131=DIRECTION('ref_axis',(0.5,0.,-0.866025403784439));
#7132=DIRECTION('center_axis',(0.,1.,0.));
#7133=DIRECTION('ref_axis',(0.,0.,1.));
#7134=DIRECTION('center_axis',(0.,-1.,0.));
#7135=DIRECTION('ref_axis',(1.,0.,0.));
#7136=DIRECTION('center_axis',(0.,-1.,0.));
#7137=DIRECTION('ref_axis',(1.,0.,0.));
#7138=DIRECTION('',(0.,1.,0.));
#7139=DIRECTION('center_axis',(0.,-1.,0.));
#7140=DIRECTION('ref_axis',(1.,0.,0.));
#7141=DIRECTION('center_axis',(0.,1.,0.));
#7142=DIRECTION('ref_axis',(0.,0.,1.));
#7143=DIRECTION('center_axis',(0.,-1.,0.));
#7144=DIRECTION('ref_axis',(1.,0.,0.));
#7145=DIRECTION('center_axis',(0.,-1.,0.));
#7146=DIRECTION('ref_axis',(1.,0.,0.));
#7147=DIRECTION('',(0.,1.,0.));
#7148=DIRECTION('center_axis',(0.,-1.,0.));
#7149=DIRECTION('ref_axis',(1.,0.,0.));
#7150=DIRECTION('center_axis',(0.,-1.,0.));
#7151=DIRECTION('ref_axis',(1.,0.,0.));
#7152=DIRECTION('',(0.,1.,0.));
#7153=DIRECTION('center_axis',(0.,-1.,0.));
#7154=DIRECTION('ref_axis',(0.,0.,-1.));
#7155=DIRECTION('center_axis',(0.,-1.,0.));
#7156=DIRECTION('ref_axis',(1.,0.,0.));
#7157=DIRECTION('center_axis',(0.,-1.,0.));
#7158=DIRECTION('ref_axis',(1.,0.,0.));
#7159=DIRECTION('',(0.,1.,0.));
#7160=DIRECTION('axis',(0.,0.,1.));
#7161=DIRECTION('refdir',(1.,0.,0.));
#7162=DIRECTION('center_axis',(0.,1.,0.));
#7163=DIRECTION('ref_axis',(0.,0.,1.));
#7164=DIRECTION('center_axis',(0.,-1.,0.));
#7165=DIRECTION('ref_axis',(1.,0.,0.));
#7166=DIRECTION('center_axis',(0.,-1.,0.));
#7167=DIRECTION('ref_axis',(1.,0.,0.));
#7168=DIRECTION('center_axis',(0.,-1.,0.));
#7169=DIRECTION('ref_axis',(1.,0.,0.));
#7170=DIRECTION('center_axis',(0.,-1.,0.));
#7171=DIRECTION('ref_axis',(1.,0.,0.));
#7172=DIRECTION('',(0.,1.,0.));
#7173=DIRECTION('center_axis',(0.,-1.,0.));
#7174=DIRECTION('ref_axis',(0.,0.,-1.));
#7175=DIRECTION('center_axis',(0.,-1.,0.));
#7176=DIRECTION('ref_axis',(1.,0.,0.));
#7177=DIRECTION('center_axis',(0.,-1.,0.));
#7178=DIRECTION('ref_axis',(1.,0.,0.));
#7179=DIRECTION('center_axis',(0.,-1.,0.));
#7180=DIRECTION('ref_axis',(1.,0.,0.));
#7181=DIRECTION('',(0.,1.,0.));
#7182=DIRECTION('center_axis',(0.,-1.,0.));
#7183=DIRECTION('ref_axis',(0.,0.,-1.));
#7184=DIRECTION('center_axis',(0.,-1.,0.));
#7185=DIRECTION('ref_axis',(1.,0.,0.));
#7186=DIRECTION('center_axis',(0.,-1.,0.));
#7187=DIRECTION('ref_axis',(1.,0.,0.));
#7188=DIRECTION('',(0.,1.,0.));
#7189=DIRECTION('',(0.,0.,1.));
#7190=DIRECTION('',(1.,0.,0.));
#7191=DIRECTION('',(0.,0.,1.));
#7192=DIRECTION('',(1.,0.,0.));
#7193=DIRECTION('axis',(0.,0.,1.));
#7194=DIRECTION('refdir',(1.,0.,0.));
#7195=DIRECTION('center_axis',(0.,1.,0.));
#7196=DIRECTION('ref_axis',(1.,0.,0.));
#7197=DIRECTION('center_axis',(0.,1.,0.));
#7198=DIRECTION('ref_axis',(1.,0.,0.));
#7199=DIRECTION('',(0.707106781186548,-0.707106781186547,-8.65956056235494E-17));
#7200=DIRECTION('center_axis',(0.,-1.,0.));
#7201=DIRECTION('ref_axis',(1.,0.,0.));
#7202=DIRECTION('center_axis',(0.,1.,0.));
#7203=DIRECTION('ref_axis',(1.,0.,0.));
#7204=DIRECTION('',(0.,-1.,0.));
#7205=DIRECTION('center_axis',(0.,-1.,0.));
#7206=DIRECTION('ref_axis',(1.,0.,0.));
#7207=DIRECTION('center_axis',(0.,1.,0.));
#7208=DIRECTION('ref_axis',(1.,0.,0.));
#7209=DIRECTION('center_axis',(0.,1.,0.));
#7210=DIRECTION('ref_axis',(1.,0.,0.));
#7211=DIRECTION('center_axis',(0.,1.,0.));
#7212=DIRECTION('ref_axis',(1.,0.,0.));
#7213=DIRECTION('',(0.,-1.,0.));
#7214=DIRECTION('center_axis',(0.,1.,0.));
#7215=DIRECTION('ref_axis',(1.,0.,0.));
#7216=DIRECTION('center_axis',(0.,1.,0.));
#7217=DIRECTION('ref_axis',(1.,0.,0.));
#7218=DIRECTION('axis',(0.,0.,1.));
#7219=DIRECTION('refdir',(1.,0.,0.));
#7220=DIRECTION('center_axis',(0.,1.,0.));
#7221=DIRECTION('ref_axis',(1.,0.,0.));
#7222=DIRECTION('',(0.866025403784439,-0.5,1.06057523872491E-16));
#7223=DIRECTION('center_axis',(0.,-1.,0.));
#7224=DIRECTION('ref_axis',(1.,0.,0.));
#7225=DIRECTION('center_axis',(0.,-1.,0.));
#7226=DIRECTION('ref_axis',(1.,0.,0.));
#7227=DIRECTION('center_axis',(0.,1.,0.));
#7228=DIRECTION('ref_axis',(1.,0.,0.));
#7229=DIRECTION('',(-0.866025403784439,-0.5,-1.06057523872491E-16));
#7230=DIRECTION('center_axis',(1.20185167898973E-16,0.,-1.));
#7231=DIRECTION('ref_axis',(-1.,0.,-1.20185167898973E-16));
#7232=DIRECTION('',(0.,1.,0.));
#7233=DIRECTION('',(0.,1.,0.));
#7234=DIRECTION('center_axis',(-0.866025403784439,0.,-0.5));
#7235=DIRECTION('ref_axis',(-0.5,0.,0.866025403784439));
#7236=DIRECTION('',(0.,1.,0.));
#7237=DIRECTION('center_axis',(-0.866025403784439,0.,0.5));
#7238=DIRECTION('ref_axis',(0.5,0.,0.866025403784439));
#7239=DIRECTION('',(0.,1.,0.));
#7240=DIRECTION('center_axis',(0.,1.,0.));
#7241=DIRECTION('ref_axis',(1.,0.,0.));
#7242=DIRECTION('center_axis',(0.,1.,0.));
#7243=DIRECTION('ref_axis',(1.,0.,0.));
#7244=DIRECTION('',(0.,-1.,0.));
#7245=DIRECTION('center_axis',(0.,1.,0.));
#7246=DIRECTION('ref_axis',(1.,0.,0.));
#7247=DIRECTION('center_axis',(-2.40370335797945E-16,0.,1.));
#7248=DIRECTION('ref_axis',(1.,0.,2.40370335797945E-16));
#7249=DIRECTION('',(0.,1.,0.));
#7250=DIRECTION('center_axis',(0.866025403784439,0.,-0.5));
#7251=DIRECTION('ref_axis',(-0.5,0.,-0.866025403784439));
#7252=DIRECTION('',(0.,1.,0.));
#7253=DIRECTION('center_axis',(0.866025403784439,0.,0.5));
#7254=DIRECTION('ref_axis',(0.5,0.,-0.866025403784439));
#7255=DIRECTION('center_axis',(0.,1.,0.));
#7256=DIRECTION('ref_axis',(1.,0.,0.));
#7257=DIRECTION('center_axis',(0.,1.,0.));
#7258=DIRECTION('ref_axis',(1.,0.,0.));
#7259=DIRECTION('axis',(0.,0.,1.));
#7260=DIRECTION('refdir',(1.,0.,0.));
#7261=DIRECTION('axis',(0.,0.,1.));
#7262=DIRECTION('refdir',(1.,0.,0.));
#7263=DIRECTION('center_axis',(0.,0.,1.));
#7264=DIRECTION('ref_axis',(1.,0.,0.));
#7265=DIRECTION('center_axis',(0.,0.,1.));
#7266=DIRECTION('ref_axis',(1.,0.,0.));
#7267=DIRECTION('',(0.,0.,1.));
#7268=DIRECTION('center_axis',(0.,0.,-1.));
#7269=DIRECTION('ref_axis',(1.,0.,0.));
#7270=DIRECTION('center_axis',(0.,0.,1.));
#7271=DIRECTION('ref_axis',(1.,0.,0.));
#7272=DIRECTION('center_axis',(0.,0.,1.));
#7273=DIRECTION('ref_axis',(1.,0.,0.));
#7274=DIRECTION('center_axis',(0.,0.,1.));
#7275=DIRECTION('ref_axis',(1.,0.,0.));
#7276=DIRECTION('center_axis',(0.,0.,1.));
#7277=DIRECTION('ref_axis',(1.,0.,0.));
#7278=DIRECTION('',(0.,0.,1.));
#7279=DIRECTION('center_axis',(-1.,0.,0.));
#7280=DIRECTION('ref_axis',(0.,-1.,0.));
#7281=DIRECTION('',(0.,0.,-1.));
#7282=DIRECTION('',(0.,-1.,0.));
#7283=DIRECTION('',(0.,0.,1.));
#7284=DIRECTION('',(0.,-1.,0.));
#7285=DIRECTION('center_axis',(0.,1.,0.));
#7286=DIRECTION('ref_axis',(-1.,0.,0.));
#7287=DIRECTION('',(-1.,0.,0.));
#7288=DIRECTION('',(-1.,0.,0.));
#7289=DIRECTION('',(0.,0.,1.));
#7290=DIRECTION('center_axis',(1.,0.,0.));
#7291=DIRECTION('ref_axis',(0.,1.,0.));
#7292=DIRECTION('',(0.,1.,0.));
#7293=DIRECTION('',(0.,1.,0.));
#7294=DIRECTION('',(0.,0.,1.));
#7295=DIRECTION('center_axis',(0.,-1.,0.));
#7296=DIRECTION('ref_axis',(1.,0.,0.));
#7297=DIRECTION('',(0.,0.,1.));
#7298=DIRECTION('',(1.,0.,0.));
#7299=DIRECTION('',(1.,0.,0.));
#7300=DIRECTION('center_axis',(0.,0.,1.));
#7301=DIRECTION('ref_axis',(1.,0.,0.));
#7302=DIRECTION('',(0.,1.,0.));
#7303=DIRECTION('',(-1.,0.,0.));
#7304=DIRECTION('center_axis',(1.,0.,0.));
#7305=DIRECTION('ref_axis',(0.,1.,0.));
#7306=DIRECTION('',(0.,0.,1.));
#7307=DIRECTION('',(0.,1.,0.));
#7308=DIRECTION('',(0.,0.,1.));
#7309=DIRECTION('',(0.,1.,0.));
#7310=DIRECTION('center_axis',(0.,1.,0.));
#7311=DIRECTION('ref_axis',(-1.,0.,0.));
#7312=DIRECTION('',(-1.,0.,0.));
#7313=DIRECTION('',(-1.,0.,0.));
#7314=DIRECTION('',(0.,0.,1.));
#7315=DIRECTION('',(-1.,0.,0.));
#7316=DIRECTION('',(0.,0.,-1.));
#7317=DIRECTION('',(-1.,0.,0.));
#7318=DIRECTION('',(-1.,0.,0.));
#7319=DIRECTION('',(0.,0.,1.));
#7320=DIRECTION('',(-1.,0.,0.));
#7321=DIRECTION('center_axis',(1.,0.,0.));
#7322=DIRECTION('ref_axis',(0.,0.,-1.));
#7323=DIRECTION('',(0.,0.,1.));
#7324=DIRECTION('center_axis',(1.,0.,0.));
#7325=DIRECTION('ref_axis',(0.,0.,-1.));
#7326=DIRECTION('center_axis',(1.,0.,0.));
#7327=DIRECTION('ref_axis',(0.,0.,-1.));
#7328=DIRECTION('center_axis',(1.,0.,0.));
#7329=DIRECTION('ref_axis',(0.,0.,-1.));
#7330=DIRECTION('',(1.,0.,0.));
#7331=DIRECTION('center_axis',(1.,0.,0.));
#7332=DIRECTION('ref_axis',(0.,0.,-1.));
#7333=DIRECTION('',(0.,0.,-1.));
#7334=DIRECTION('center_axis',(0.,0.,1.));
#7335=DIRECTION('ref_axis',(1.,0.,0.));
#7336=DIRECTION('center_axis',(0.,0.,1.));
#7337=DIRECTION('ref_axis',(1.,0.,0.));
#7338=DIRECTION('',(1.,0.,0.));
#7339=DIRECTION('center_axis',(0.,0.,1.));
#7340=DIRECTION('ref_axis',(1.,0.,0.));
#7341=DIRECTION('center_axis',(0.,0.,1.));
#7342=DIRECTION('ref_axis',(1.,0.,0.));
#7343=DIRECTION('center_axis',(0.,0.,1.));
#7344=DIRECTION('ref_axis',(1.,0.,0.));
#7345=DIRECTION('center_axis',(0.,0.,1.));
#7346=DIRECTION('ref_axis',(1.,0.,0.));
#7347=DIRECTION('',(0.,0.,1.));
#7348=DIRECTION('',(0.,0.,1.));
#7349=DIRECTION('center_axis',(0.,0.,-1.));
#7350=DIRECTION('ref_axis',(1.,0.,0.));
#7351=DIRECTION('',(0.,0.,-1.));
#7352=DIRECTION('center_axis',(0.,0.,-1.));
#7353=DIRECTION('ref_axis',(1.,0.,0.));
#7354=DIRECTION('center_axis',(0.,-1.,0.));
#7355=DIRECTION('ref_axis',(1.,0.,0.));
#7356=DIRECTION('',(1.,0.,0.));
#7357=DIRECTION('',(1.,0.,0.));
#7358=DIRECTION('',(1.,0.,0.));
#7359=DIRECTION('',(0.,0.,1.));
#7360=DIRECTION('',(1.,0.,0.));
#7361=DIRECTION('',(1.,0.,0.));
#7362=DIRECTION('center_axis',(0.,0.,1.));
#7363=DIRECTION('ref_axis',(1.,0.,0.));
#7364=DIRECTION('center_axis',(0.,0.,1.));
#7365=DIRECTION('ref_axis',(1.,0.,0.));
#7366=DIRECTION('center_axis',(0.,0.,1.));
#7367=DIRECTION('ref_axis',(1.,0.,0.));
#7368=DIRECTION('center_axis',(0.,0.,1.));
#7369=DIRECTION('ref_axis',(1.,0.,0.));
#7370=DIRECTION('center_axis',(0.,0.,1.));
#7371=DIRECTION('ref_axis',(1.,0.,0.));
#7372=DIRECTION('center_axis',(0.,0.,1.));
#7373=DIRECTION('ref_axis',(1.,0.,0.));
#7374=DIRECTION('center_axis',(0.,0.,1.));
#7375=DIRECTION('ref_axis',(1.,0.,0.));
#7376=DIRECTION('center_axis',(0.,0.,1.));
#7377=DIRECTION('ref_axis',(1.,0.,0.));
#7378=DIRECTION('',(0.,0.,-1.));
#7379=DIRECTION('center_axis',(0.,0.,1.));
#7380=DIRECTION('ref_axis',(1.,0.,0.));
#7381=DIRECTION('center_axis',(0.,0.,1.));
#7382=DIRECTION('ref_axis',(1.,0.,0.));
#7383=DIRECTION('center_axis',(0.,0.,1.));
#7384=DIRECTION('ref_axis',(1.,0.,0.));
#7385=DIRECTION('',(0.,-1.,0.));
#7386=DIRECTION('center_axis',(0.,0.,1.));
#7387=DIRECTION('ref_axis',(1.,0.,0.));
#7388=DIRECTION('center_axis',(-1.,0.,0.));
#7389=DIRECTION('ref_axis',(0.,-1.,0.));
#7390=DIRECTION('',(0.,-1.,0.));
#7391=DIRECTION('center_axis',(0.,0.,1.));
#7392=DIRECTION('ref_axis',(1.,0.,0.));
#7393=DIRECTION('axis',(0.,0.,1.));
#7394=DIRECTION('refdir',(1.,0.,0.));
#7395=DIRECTION('center_axis',(0.,0.,1.));
#7396=DIRECTION('ref_axis',(1.,0.,0.));
#7397=DIRECTION('center_axis',(0.,0.,1.));
#7398=DIRECTION('ref_axis',(1.,0.,0.));
#7399=DIRECTION('',(0.,0.,1.));
#7400=DIRECTION('center_axis',(0.,0.,-1.));
#7401=DIRECTION('ref_axis',(1.,0.,0.));
#7402=DIRECTION('center_axis',(0.,0.,1.));
#7403=DIRECTION('ref_axis',(1.,0.,0.));
#7404=DIRECTION('center_axis',(0.,0.,1.));
#7405=DIRECTION('ref_axis',(1.,0.,0.));
#7406=DIRECTION('center_axis',(0.,0.,1.));
#7407=DIRECTION('ref_axis',(1.,0.,0.));
#7408=DIRECTION('',(0.,0.,1.));
#7409=DIRECTION('center_axis',(0.,0.,1.));
#7410=DIRECTION('ref_axis',(1.,0.,0.));
#7411=DIRECTION('center_axis',(0.,0.,1.));
#7412=DIRECTION('ref_axis',(1.,0.,0.));
#7413=DIRECTION('center_axis',(0.,0.,1.));
#7414=DIRECTION('ref_axis',(1.,0.,0.));
#7415=DIRECTION('center_axis',(0.,0.,1.));
#7416=DIRECTION('ref_axis',(1.,0.,0.));
#7417=DIRECTION('',(0.,0.,-1.));
#7418=DIRECTION('center_axis',(0.,0.,1.));
#7419=DIRECTION('ref_axis',(1.,0.,0.));
#7420=DIRECTION('center_axis',(0.,0.,1.));
#7421=DIRECTION('ref_axis',(1.,0.,0.));
#7422=DIRECTION('center_axis',(0.,0.,1.));
#7423=DIRECTION('ref_axis',(1.,0.,0.));
#7424=DIRECTION('axis',(0.,0.,1.));
#7425=DIRECTION('refdir',(1.,0.,0.));
#7426=DIRECTION('center_axis',(0.,0.,1.));
#7427=DIRECTION('ref_axis',(1.,0.,0.));
#7428=DIRECTION('center_axis',(0.,0.,-1.));
#7429=DIRECTION('ref_axis',(1.,0.,0.));
#7430=DIRECTION('',(0.,0.,1.));
#7431=DIRECTION('center_axis',(0.,0.,-1.));
#7432=DIRECTION('ref_axis',(1.,0.,0.));
#7433=DIRECTION('center_axis',(0.,0.,1.));
#7434=DIRECTION('ref_axis',(1.,0.,0.));
#7435=DIRECTION('center_axis',(0.,0.,1.));
#7436=DIRECTION('ref_axis',(1.,0.,0.));
#7437=DIRECTION('center_axis',(0.,0.,1.));
#7438=DIRECTION('ref_axis',(1.,0.,0.));
#7439=DIRECTION('center_axis',(0.,0.,-1.));
#7440=DIRECTION('ref_axis',(1.,0.,0.));
#7441=DIRECTION('center_axis',(0.,0.,1.));
#7442=DIRECTION('ref_axis',(1.,0.,0.));
#7443=DIRECTION('',(0.,0.,-1.));
#7444=DIRECTION('center_axis',(0.,0.,1.));
#7445=DIRECTION('ref_axis',(1.,0.,0.));
#7446=DIRECTION('center_axis',(0.,0.,1.));
#7447=DIRECTION('ref_axis',(1.,0.,0.));
#7448=DIRECTION('center_axis',(0.,0.,-1.));
#7449=DIRECTION('ref_axis',(1.,0.,0.));
#7450=DIRECTION('',(0.,0.,-1.));
#7451=DIRECTION('center_axis',(0.,0.,-1.));
#7452=DIRECTION('ref_axis',(1.,0.,0.));
#7453=DIRECTION('center_axis',(0.,0.,1.));
#7454=DIRECTION('ref_axis',(1.,0.,0.));
#7455=DIRECTION('center_axis',(0.,0.,1.));
#7456=DIRECTION('ref_axis',(1.,0.,0.));
#7457=DIRECTION('',(0.,0.,-1.));
#7458=DIRECTION('center_axis',(0.,0.,1.));
#7459=DIRECTION('ref_axis',(1.,0.,0.));
#7460=DIRECTION('center_axis',(0.,0.,1.));
#7461=DIRECTION('ref_axis',(1.,0.,0.));
#7462=DIRECTION('axis',(0.,0.,1.));
#7463=DIRECTION('refdir',(1.,0.,0.));
#7464=DIRECTION('center_axis',(0.,0.,1.));
#7465=DIRECTION('ref_axis',(1.,0.,0.));
#7466=DIRECTION('center_axis',(0.,0.,-1.));
#7467=DIRECTION('ref_axis',(1.,0.,0.));
#7468=DIRECTION('',(0.,0.,-1.));
#7469=DIRECTION('center_axis',(0.,0.,-1.));
#7470=DIRECTION('ref_axis',(1.,0.,0.));
#7471=DIRECTION('center_axis',(0.,0.,1.));
#7472=DIRECTION('ref_axis',(1.,0.,0.));
#7473=DIRECTION('center_axis',(0.,0.,1.));
#7474=DIRECTION('ref_axis',(1.,0.,0.));
#7475=DIRECTION('',(0.,0.,-1.));
#7476=DIRECTION('center_axis',(0.,0.,1.));
#7477=DIRECTION('ref_axis',(1.,0.,0.));
#7478=DIRECTION('center_axis',(0.,0.,1.));
#7479=DIRECTION('ref_axis',(1.,0.,0.));
#7480=DIRECTION('center_axis',(0.,0.,1.));
#7481=DIRECTION('ref_axis',(1.,0.,0.));
#7482=DIRECTION('axis',(0.,0.,1.));
#7483=DIRECTION('refdir',(1.,0.,0.));
#7484=DIRECTION('center_axis',(1.,0.,0.));
#7485=DIRECTION('ref_axis',(0.,0.,-1.));
#7486=DIRECTION('center_axis',(-1.,0.,0.));
#7487=DIRECTION('ref_axis',(0.,0.,-1.));
#7488=DIRECTION('center_axis',(1.,0.,0.));
#7489=DIRECTION('ref_axis',(0.,0.,-1.));
#7490=DIRECTION('center_axis',(-1.,0.,0.));
#7491=DIRECTION('ref_axis',(0.,0.,-1.));
#7492=DIRECTION('',(-0.707106781186548,8.65956056235493E-17,-0.707106781186547));
#7493=DIRECTION('center_axis',(1.,0.,0.));
#7494=DIRECTION('ref_axis',(0.,0.,-1.));
#7495=DIRECTION('center_axis',(1.,0.,0.));
#7496=DIRECTION('ref_axis',(0.,0.,-1.));
#7497=DIRECTION('',(-1.,0.,0.));
#7498=DIRECTION('center_axis',(1.,0.,0.));
#7499=DIRECTION('ref_axis',(0.,0.,-1.));
#7500=DIRECTION('axis',(0.,0.,1.));
#7501=DIRECTION('refdir',(1.,0.,0.));
#7502=DIRECTION('center_axis',(0.,1.,0.));
#7503=DIRECTION('ref_axis',(1.,0.,0.));
#7504=DIRECTION('center_axis',(0.,1.,0.));
#7505=DIRECTION('ref_axis',(1.,0.,0.));
#7506=DIRECTION('center_axis',(0.866025403784439,0.,-0.5));
#7507=DIRECTION('ref_axis',(0.5,0.,0.866025403784439));
#7508=DIRECTION('',(0.5,0.,0.866025403784439));
#7509=DIRECTION('',(0.,-1.,0.));
#7510=DIRECTION('',(0.5,0.,0.866025403784439));
#7511=DIRECTION('',(0.,-1.,0.));
#7512=DIRECTION('center_axis',(1.20185167898973E-16,0.,-1.));
#7513=DIRECTION('ref_axis',(1.,0.,1.20185167898973E-16));
#7514=DIRECTION('',(1.,0.,1.20185167898973E-16));
#7515=DIRECTION('',(0.,-1.,0.));
#7516=DIRECTION('',(1.,0.,1.20185167898973E-16));
#7517=DIRECTION('center_axis',(-0.866025403784439,0.,-0.5));
#7518=DIRECTION('ref_axis',(0.5,0.,-0.866025403784439));
#7519=DIRECTION('',(0.5,0.,-0.866025403784439));
#7520=DIRECTION('',(0.,-1.,0.));
#7521=DIRECTION('',(0.5,0.,-0.866025403784439));
#7522=DIRECTION('center_axis',(-0.866025403784439,0.,0.5));
#7523=DIRECTION('ref_axis',(-0.5,0.,-0.866025403784439));
#7524=DIRECTION('',(-0.5,0.,-0.866025403784439));
#7525=DIRECTION('',(0.,-1.,0.));
#7526=DIRECTION('',(-0.5,0.,-0.866025403784439));
#7527=DIRECTION('center_axis',(-2.40370335797945E-16,0.,1.));
#7528=DIRECTION('ref_axis',(-1.,0.,-2.40370335797945E-16));
#7529=DIRECTION('',(-1.,0.,-2.40370335797945E-16));
#7530=DIRECTION('',(0.,-1.,0.));
#7531=DIRECTION('',(-1.,0.,-2.40370335797945E-16));
#7532=DIRECTION('center_axis',(0.866025403784439,0.,0.5));
#7533=DIRECTION('ref_axis',(-0.5,0.,0.866025403784439));
#7534=DIRECTION('',(-0.5,0.,0.866025403784439));
#7535=DIRECTION('',(-0.5,0.,0.866025403784439));
#7536=DIRECTION('center_axis',(0.,-1.,0.));
#7537=DIRECTION('ref_axis',(0.,0.,-1.));
#7538=DIRECTION('center_axis',(0.,1.,0.));
#7539=DIRECTION('ref_axis',(0.,0.,1.));
#7540=DIRECTION('center_axis',(0.,-1.,0.));
#7541=DIRECTION('ref_axis',(1.,0.,0.));
#7542=DIRECTION('center_axis',(0.,-1.,0.));
#7543=DIRECTION('ref_axis',(1.,0.,0.));
#7544=DIRECTION('center_axis',(0.,-1.,0.));
#7545=DIRECTION('ref_axis',(1.,0.,0.));
#7546=DIRECTION('',(0.707106781186548,0.707106781186547,8.65956056235494E-17));
#7547=DIRECTION('center_axis',(0.,-1.,0.));
#7548=DIRECTION('ref_axis',(1.,0.,0.));
#7549=DIRECTION('',(0.,1.,0.));
#7550=DIRECTION('axis',(0.,0.,1.));
#7551=DIRECTION('refdir',(1.,0.,0.));
#7552=DIRECTION('center_axis',(0.,1.,0.));
#7553=DIRECTION('ref_axis',(0.,0.,1.));
#7554=DIRECTION('center_axis',(0.,-1.,0.));
#7555=DIRECTION('ref_axis',(1.,0.,0.));
#7556=DIRECTION('center_axis',(0.,-1.,0.));
#7557=DIRECTION('ref_axis',(1.,0.,0.));
#7558=DIRECTION('center_axis',(0.,-1.,0.));
#7559=DIRECTION('ref_axis',(1.,0.,0.));
#7560=DIRECTION('',(0.707106781186547,0.707106781186548,8.65956056235493E-17));
#7561=DIRECTION('center_axis',(0.,-1.,0.));
#7562=DIRECTION('ref_axis',(1.,0.,0.));
#7563=DIRECTION('center_axis',(0.,-1.,0.));
#7564=DIRECTION('ref_axis',(1.,0.,0.));
#7565=DIRECTION('',(0.,1.,0.));
#7566=DIRECTION('center_axis',(0.,1.,0.));
#7567=DIRECTION('ref_axis',(1.,0.,0.));
#7568=DIRECTION('center_axis',(0.,-1.,0.));
#7569=DIRECTION('ref_axis',(1.,0.,0.));
#7570=DIRECTION('',(-0.707106781186547,0.707106781186548,-8.65956056235493E-17));
#7571=DIRECTION('center_axis',(0.,-1.,0.));
#7572=DIRECTION('ref_axis',(0.,0.,-1.));
#7573=DIRECTION('center_axis',(0.,-1.,0.));
#7574=DIRECTION('ref_axis',(1.,0.,0.));
#7575=DIRECTION('center_axis',(0.,1.,0.));
#7576=DIRECTION('ref_axis',(1.,0.,0.));
#7577=DIRECTION('center_axis',(0.,1.,0.));
#7578=DIRECTION('ref_axis',(1.,0.,0.));
#7579=DIRECTION('',(-0.447213595499958,0.894427190999916,-5.47678698264203E-17));
#7580=DIRECTION('center_axis',(0.,-1.,0.));
#7581=DIRECTION('ref_axis',(1.,0.,0.));
#7582=DIRECTION('center_axis',(0.,1.,0.));
#7583=DIRECTION('ref_axis',(1.,0.,0.));
#7584=DIRECTION('',(0.,1.,0.));
#7585=DIRECTION('center_axis',(0.,1.,0.));
#7586=DIRECTION('ref_axis',(1.,0.,0.));
#7587=DIRECTION('center_axis',(0.,-1.,0.));
#7588=DIRECTION('ref_axis',(1.,0.,0.));
#7589=DIRECTION('',(-0.707106781186547,0.707106781186548,-8.65956056235493E-17));
#7590=DIRECTION('center_axis',(0.,-1.,0.));
#7591=DIRECTION('ref_axis',(0.,0.,-1.));
#7592=DIRECTION('center_axis',(0.866025403784439,0.,-0.5));
#7593=DIRECTION('ref_axis',(0.5,0.,0.866025403784439));
#7594=DIRECTION('',(-0.5,0.,-0.866025403784439));
#7595=DIRECTION('',(0.,-1.,0.));
#7596=DIRECTION('',(0.5,0.,0.866025403784439));
#7597=DIRECTION('',(0.,-1.,0.));
#7598=DIRECTION('center_axis',(1.60246890531964E-16,0.,-1.));
#7599=DIRECTION('ref_axis',(1.,0.,1.60246890531964E-16));
#7600=DIRECTION('',(-1.,0.,-1.60246890531964E-16));
#7601=DIRECTION('',(0.,-1.,0.));
#7602=DIRECTION('',(1.,0.,1.60246890531964E-16));
#7603=DIRECTION('center_axis',(-0.866025403784439,0.,-0.5));
#7604=DIRECTION('ref_axis',(0.5,0.,-0.866025403784439));
#7605=DIRECTION('',(-0.5,0.,0.866025403784439));
#7606=DIRECTION('',(0.,-1.,0.));
#7607=DIRECTION('',(0.5,0.,-0.866025403784439));
#7608=DIRECTION('center_axis',(-0.866025403784439,0.,0.5));
#7609=DIRECTION('ref_axis',(-0.5,0.,-0.866025403784439));
#7610=DIRECTION('',(0.5,0.,0.866025403784439));
#7611=DIRECTION('',(0.,-1.,0.));
#7612=DIRECTION('',(-0.5,0.,-0.866025403784439));
#7613=DIRECTION('center_axis',(-1.60246890531964E-16,0.,1.));
#7614=DIRECTION('ref_axis',(-1.,0.,-1.60246890531964E-16));
#7615=DIRECTION('',(1.,0.,1.60246890531964E-16));
#7616=DIRECTION('',(0.,-1.,0.));
#7617=DIRECTION('',(-1.,0.,-1.60246890531964E-16));
#7618=DIRECTION('center_axis',(0.866025403784439,0.,0.5));
#7619=DIRECTION('ref_axis',(-0.5,0.,0.866025403784439));
#7620=DIRECTION('',(0.5,0.,-0.866025403784439));
#7621=DIRECTION('',(-0.5,0.,0.866025403784439));
#7622=DIRECTION('center_axis',(0.,1.,0.));
#7623=DIRECTION('ref_axis',(1.,0.,0.));
#7624=DIRECTION('center_axis',(0.,-1.,0.));
#7625=DIRECTION('ref_axis',(0.,0.,-1.));
#7626=DIRECTION('',(0.,0.,1.));
#7627=DIRECTION('',(1.,0.,0.));
#7628=DIRECTION('',(0.,0.,1.));
#7629=DIRECTION('',(1.,0.,0.));
#7630=DIRECTION('',(0.,0.,1.));
#7631=DIRECTION('',(1.,0.,0.));
#7632=DIRECTION('',(0.,0.,1.));
#7633=DIRECTION('',(1.,0.,0.));
#7634=DIRECTION('',(0.,0.,1.));
#7635=DIRECTION('',(1.,0.,0.));
#7636=DIRECTION('',(0.,0.,1.));
#7637=DIRECTION('',(1.,0.,0.));
#7638=DIRECTION('',(0.,0.,1.));
#7639=DIRECTION('',(1.,0.,0.));
#7640=DIRECTION('',(0.,0.,1.));
#7641=DIRECTION('',(1.,0.,0.));
#7642=DIRECTION('',(0.,0.,1.));
#7643=DIRECTION('',(1.,0.,0.));
#7644=DIRECTION('',(0.,0.,1.));
#7645=DIRECTION('',(1.,0.,0.));
#7646=DIRECTION('',(0.,0.,1.));
#7647=DIRECTION('',(1.,0.,0.));
#7648=DIRECTION('',(0.,0.,1.));
#7649=DIRECTION('',(1.,0.,0.));
#7650=DIRECTION('',(0.,0.,1.));
#7651=DIRECTION('',(1.,0.,0.));
#7652=DIRECTION('',(0.,0.,1.));
#7653=DIRECTION('',(1.,0.,0.));
#7654=DIRECTION('',(0.,0.,1.));
#7655=DIRECTION('',(1.,0.,0.));
#7656=DIRECTION('',(0.,0.,1.));
#7657=DIRECTION('',(1.,0.,0.));
#7658=DIRECTION('',(0.,0.,1.));
#7659=DIRECTION('',(1.,0.,0.));
#7660=DIRECTION('',(0.,0.,1.));
#7661=DIRECTION('',(1.,0.,0.));
#7662=DIRECTION('',(0.,-1.,2.22044604925031E-16));
#7663=DIRECTION('',(1.,0.,0.));
#7664=DIRECTION('',(0.,1.,2.22044604925031E-16));
#7665=DIRECTION('',(1.,0.,0.));
#7666=DIRECTION('',(0.,1.,2.22044604925031E-16));
#7667=DIRECTION('',(1.,0.,0.));
#7668=DIRECTION('',(0.,1.,2.22044604925031E-16));
#7669=DIRECTION('',(1.,0.,0.));
#7670=DIRECTION('',(0.,1.,2.22044604925031E-16));
#7671=DIRECTION('',(1.,0.,0.));
#7672=DIRECTION('',(0.,-1.,2.22044604925031E-16));
#7673=DIRECTION('',(1.,0.,0.));
#7674=DIRECTION('',(0.,-1.,2.22044604925031E-16));
#7675=DIRECTION('',(1.,0.,0.));
#7676=DIRECTION('',(0.,-1.,2.22044604925031E-16));
#7677=DIRECTION('',(1.,0.,0.));
#7678=DIRECTION('',(0.,-1.,2.22044604925031E-16));
#7679=DIRECTION('',(1.,0.,0.));
#7680=DIRECTION('',(0.,1.,2.22044604925031E-16));
#7681=DIRECTION('',(1.,0.,0.));
#7682=DIRECTION('',(0.,0.,1.));
#7683=DIRECTION('',(1.,0.,0.));
#7684=DIRECTION('',(0.,0.,1.));
#7685=DIRECTION('',(1.,0.,0.));
#7686=DIRECTION('',(0.,1.,2.22044604925031E-16));
#7687=DIRECTION('',(1.,0.,0.));
#7688=DIRECTION('',(0.,-1.,2.22044604925031E-16));
#7689=DIRECTION('',(1.,0.,0.));
#7690=DIRECTION('',(0.,-1.,2.22044604925031E-16));
#7691=DIRECTION('',(1.,0.,0.));
#7692=DIRECTION('',(0.,-1.,2.22044604925031E-16));
#7693=DIRECTION('',(1.,0.,0.));
#7694=DIRECTION('',(0.,1.,2.22044604925031E-16));
#7695=DIRECTION('',(1.,0.,0.));
#7696=DIRECTION('',(0.,-1.,2.22044604925031E-16));
#7697=DIRECTION('',(1.,0.,0.));
#7698=DIRECTION('',(0.,-1.,2.22044604925031E-16));
#7699=DIRECTION('',(1.,0.,0.));
#7700=DIRECTION('',(0.,-1.,2.22044604925031E-16));
#7701=DIRECTION('',(1.,0.,0.));
#7702=DIRECTION('',(0.,1.,2.22044604925031E-16));
#7703=DIRECTION('',(1.,0.,0.));
#7704=DIRECTION('',(0.,-1.,2.22044604925031E-16));
#7705=DIRECTION('',(1.,0.,0.));
#7706=DIRECTION('',(0.,-1.,2.22044604925031E-16));
#7707=DIRECTION('',(1.,0.,0.));
#7708=DIRECTION('',(0.,-1.,2.22044604925031E-16));
#7709=DIRECTION('',(1.,0.,0.));
#7710=DIRECTION('',(0.,1.,2.22044604925031E-16));
#7711=DIRECTION('',(1.,0.,0.));
#7712=DIRECTION('',(0.,-1.,2.22044604925031E-16));
#7713=DIRECTION('',(1.,0.,0.));
#7714=DIRECTION('',(0.,-1.,2.22044604925031E-16));
#7715=DIRECTION('',(1.,0.,0.));
#7716=DIRECTION('',(0.,-1.,2.22044604925031E-16));
#7717=DIRECTION('',(1.,0.,0.));
#7718=DIRECTION('',(0.,0.,1.));
#7719=DIRECTION('',(1.,0.,0.));
#7720=DIRECTION('',(0.,0.,1.));
#7721=DIRECTION('',(1.,0.,0.));
#7722=DIRECTION('',(0.,0.,1.));
#7723=DIRECTION('',(1.,0.,0.));
#7724=DIRECTION('',(0.,0.,1.));
#7725=DIRECTION('',(1.,0.,0.));
#7726=DIRECTION('',(-1.,0.,2.22044604925031E-16));
#7727=DIRECTION('',(2.22044604925031E-16,0.,1.));
#7728=DIRECTION('',(0.,0.,1.));
#7729=DIRECTION('',(2.22044604925031E-16,-1.,0.));
#7730=DIRECTION('',(0.,-1.,2.22044604925031E-16));
#7731=DIRECTION('',(1.,0.,0.));
#7732=DIRECTION('',(0.,1.,2.22044604925031E-16));
#7733=DIRECTION('',(1.,0.,0.));
#7734=DIRECTION('',(0.,0.,1.));
#7735=DIRECTION('',(1.,0.,0.));
#7736=DIRECTION('',(0.,0.,1.));
#7737=DIRECTION('',(1.,0.,0.));
#7738=CARTESIAN_POINT('',(0.,0.,0.));
#7739=CARTESIAN_POINT('',(0.,0.,0.));
#7740=CARTESIAN_POINT('',(0.,0.,0.));
#7741=CARTESIAN_POINT('Origin',(2.72720779386421,2.72720779386421,-1.1));
#7742=CARTESIAN_POINT('',(2.45220779386421,2.72720779386421,-1.));
#7743=CARTESIAN_POINT('Origin',(2.72720779386421,2.72720779386421,-1.));
#7744=CARTESIAN_POINT('',(2.45220779386421,2.72720779386421,0.));
#7745=CARTESIAN_POINT('',(2.45220779386421,2.72720779386421,-1.1));
#7746=CARTESIAN_POINT('Origin',(2.72720779386421,2.72720779386421,0.));
#7747=CARTESIAN_POINT('Origin',(2.72720779386421,5.27279220613579,-1.1));
#7748=CARTESIAN_POINT('',(2.45220779386421,5.27279220613579,-1.));
#7749=CARTESIAN_POINT('Origin',(2.72720779386421,5.27279220613579,-1.));
#7750=CARTESIAN_POINT('',(2.45220779386421,5.27279220613579,0.));
#7751=CARTESIAN_POINT('',(2.45220779386421,5.27279220613579,-1.1));
#7752=CARTESIAN_POINT('Origin',(2.72720779386421,5.27279220613579,0.));
#7753=CARTESIAN_POINT('Origin',(5.27279220613579,5.27279220613579,-1.1));
#7754=CARTESIAN_POINT('',(4.99779220613579,5.27279220613579,-1.));
#7755=CARTESIAN_POINT('Origin',(5.27279220613579,5.27279220613579,-1.));
#7756=CARTESIAN_POINT('',(4.99779220613579,5.27279220613579,0.));
#7757=CARTESIAN_POINT('',(4.99779220613579,5.27279220613579,-1.1));
#7758=CARTESIAN_POINT('Origin',(5.27279220613579,5.27279220613579,0.));
#7759=CARTESIAN_POINT('Origin',(5.27279220613578,2.72720779386421,-1.1));
#7760=CARTESIAN_POINT('',(4.99779220613578,2.72720779386421,-1.));
#7761=CARTESIAN_POINT('Origin',(5.27279220613578,2.72720779386421,-1.));
#7762=CARTESIAN_POINT('',(4.99779220613578,2.72720779386421,0.));
#7763=CARTESIAN_POINT('',(4.99779220613578,2.72720779386421,-1.1));
#7764=CARTESIAN_POINT('Origin',(5.27279220613578,2.72720779386421,0.));
#7765=CARTESIAN_POINT('Origin',(-4.,-3.,-1.1));
#7766=CARTESIAN_POINT('',(-4.275,-3.,-1.));
#7767=CARTESIAN_POINT('Origin',(-4.,-3.,-1.));
#7768=CARTESIAN_POINT('',(-4.275,-3.,0.));
#7769=CARTESIAN_POINT('',(-4.275,-3.,-1.1));
#7770=CARTESIAN_POINT('Origin',(-4.,-3.,0.));
#7771=CARTESIAN_POINT('Origin',(1.2,-1.2,-1.1));
#7772=CARTESIAN_POINT('',(0.925,-1.2,-1.));
#7773=CARTESIAN_POINT('Origin',(1.2,-1.2,-1.));
#7774=CARTESIAN_POINT('',(0.925,-1.2,0.));
#7775=CARTESIAN_POINT('',(0.925,-1.2,-1.1));
#7776=CARTESIAN_POINT('Origin',(1.2,-1.2,0.));
#7777=CARTESIAN_POINT('Origin',(-1.2,1.2,-1.1));
#7778=CARTESIAN_POINT('',(-1.475,1.2,-1.));
#7779=CARTESIAN_POINT('Origin',(-1.2,1.2,-1.));
#7780=CARTESIAN_POINT('',(-1.475,1.2,0.));
#7781=CARTESIAN_POINT('',(-1.475,1.2,-1.1));
#7782=CARTESIAN_POINT('Origin',(-1.2,1.2,0.));
#7783=CARTESIAN_POINT('Origin',(-1.2,-1.2,-1.1));
#7784=CARTESIAN_POINT('',(-1.475,-1.2,-1.));
#7785=CARTESIAN_POINT('Origin',(-1.2,-1.2,-1.));
#7786=CARTESIAN_POINT('',(-1.475,-1.2,0.));
#7787=CARTESIAN_POINT('',(-1.475,-1.2,-1.1));
#7788=CARTESIAN_POINT('Origin',(-1.2,-1.2,0.));
#7789=CARTESIAN_POINT('Origin',(1.2,1.2,-1.1));
#7790=CARTESIAN_POINT('',(0.925,1.2,-1.));
#7791=CARTESIAN_POINT('Origin',(1.2,1.2,-1.));
#7792=CARTESIAN_POINT('',(0.925,1.2,0.));
#7793=CARTESIAN_POINT('',(0.925,1.2,-1.1));
#7794=CARTESIAN_POINT('Origin',(1.2,1.2,0.));
#7795=CARTESIAN_POINT('Origin',(7.5,7.5,-1.));
#7796=CARTESIAN_POINT('',(7.5,7.5,-1.));
#7797=CARTESIAN_POINT('',(-5.,7.5,-1.));
#7798=CARTESIAN_POINT('',(7.5,7.5,-1.));
#7799=CARTESIAN_POINT('',(-5.,7.5,0.));
#7800=CARTESIAN_POINT('',(-5.,7.5,-1.));
#7801=CARTESIAN_POINT('',(7.5,7.5,0.));
#7802=CARTESIAN_POINT('',(7.5,7.5,0.));
#7803=CARTESIAN_POINT('',(7.5,7.5,-1.));
#7804=CARTESIAN_POINT('Origin',(7.5,-3.5,-1.));
#7805=CARTESIAN_POINT('',(7.5,-3.5,-1.));
#7806=CARTESIAN_POINT('',(7.5,-3.5,-1.));
#7807=CARTESIAN_POINT('',(7.5,-3.5,0.));
#7808=CARTESIAN_POINT('',(7.5,-3.5,0.));
#7809=CARTESIAN_POINT('',(7.5,-3.5,-1.));
#7810=CARTESIAN_POINT('Origin',(-5.,-3.5,-1.));
#7811=CARTESIAN_POINT('',(-5.,-3.5,-1.));
#7812=CARTESIAN_POINT('',(-5.,-3.5,-1.));
#7813=CARTESIAN_POINT('',(-5.,-3.5,0.));
#7814=CARTESIAN_POINT('',(-5.,-3.5,0.));
#7815=CARTESIAN_POINT('',(-5.,-3.5,-1.));
#7816=CARTESIAN_POINT('Origin',(-5.,7.5,-1.));
#7817=CARTESIAN_POINT('',(-5.,7.5,-1.));
#7818=CARTESIAN_POINT('',(-5.,7.5,0.));
#7819=CARTESIAN_POINT('Origin',(1.25,2.,0.));
#7820=CARTESIAN_POINT('Origin',(1.25,2.,-1.));
#7821=CARTESIAN_POINT('',(0.,0.,0.));
#7822=CARTESIAN_POINT('Origin',(-4.5,7.5,-2.2));
#7823=CARTESIAN_POINT('',(-4.5,7.5,-2.2));
#7824=CARTESIAN_POINT('',(-5.,7.5,-2.2));
#7825=CARTESIAN_POINT('',(-4.5,7.5,-2.2));
#7826=CARTESIAN_POINT('',(-5.,7.5,-1.));
#7827=CARTESIAN_POINT('',(-5.,7.5,-2.2));
#7828=CARTESIAN_POINT('',(-4.5,7.5,-1.));
#7829=CARTESIAN_POINT('',(-4.5,7.5,-1.));
#7830=CARTESIAN_POINT('',(-4.5,7.5,-2.2));
#7831=CARTESIAN_POINT('Origin',(-4.5,-3.5,-2.2));
#7832=CARTESIAN_POINT('',(-4.5,-3.5,-2.2));
#7833=CARTESIAN_POINT('',(-4.5,-3.5,-2.2));
#7834=CARTESIAN_POINT('',(-4.5,-3.5,-1.));
#7835=CARTESIAN_POINT('',(-4.5,-3.5,-1.));
#7836=CARTESIAN_POINT('',(-4.5,-3.5,-2.2));
#7837=CARTESIAN_POINT('Origin',(-5.,-3.5,-2.2));
#7838=CARTESIAN_POINT('',(-5.,-3.5,-2.2));
#7839=CARTESIAN_POINT('',(-5.,-3.5,-2.2));
#7840=CARTESIAN_POINT('',(-5.,-3.5,-1.));
#7841=CARTESIAN_POINT('',(-5.,-3.5,-1.));
#7842=CARTESIAN_POINT('',(-5.,-3.5,-2.2));
#7843=CARTESIAN_POINT('Origin',(-5.,7.5,-2.2));
#7844=CARTESIAN_POINT('',(-5.,7.5,-2.2));
#7845=CARTESIAN_POINT('',(-5.,7.5,-1.));
#7846=CARTESIAN_POINT('Origin',(-4.75,2.,-1.));
#7847=CARTESIAN_POINT('Origin',(-4.75,2.,-2.2));
#7848=CARTESIAN_POINT('',(0.,0.,0.));
#7849=CARTESIAN_POINT('Origin',(7.5,7.5,-2.2));
#7850=CARTESIAN_POINT('',(7.5,7.5,-2.2));
#7851=CARTESIAN_POINT('',(7.,7.5,-2.2));
#7852=CARTESIAN_POINT('',(7.5,7.5,-2.2));
#7853=CARTESIAN_POINT('',(7.,7.5,-1.));
#7854=CARTESIAN_POINT('',(7.,7.5,-2.2));
#7855=CARTESIAN_POINT('',(7.5,7.5,-1.));
#7856=CARTESIAN_POINT('',(7.5,7.5,-1.));
#7857=CARTESIAN_POINT('',(7.5,7.5,-2.2));
#7858=CARTESIAN_POINT('Origin',(7.5,-3.5,-2.2));
#7859=CARTESIAN_POINT('',(7.5,-3.5,-2.2));
#7860=CARTESIAN_POINT('',(7.5,-3.5,-2.2));
#7861=CARTESIAN_POINT('',(7.5,-3.5,-1.));
#7862=CARTESIAN_POINT('',(7.5,-3.5,-1.));
#7863=CARTESIAN_POINT('',(7.5,-3.5,-2.2));
#7864=CARTESIAN_POINT('Origin',(7.,-3.5,-2.2));
#7865=CARTESIAN_POINT('',(7.,-3.5,-2.2));
#7866=CARTESIAN_POINT('',(7.,-3.5,-2.2));
#7867=CARTESIAN_POINT('',(7.,-3.5,-1.));
#7868=CARTESIAN_POINT('',(7.,-3.5,-1.));
#7869=CARTESIAN_POINT('',(7.,-3.5,-2.2));
#7870=CARTESIAN_POINT('Origin',(7.,7.5,-2.2));
#7871=CARTESIAN_POINT('',(7.,7.5,-2.2));
#7872=CARTESIAN_POINT('',(7.,7.5,-1.));
#7873=CARTESIAN_POINT('Origin',(7.25,2.,-1.));
#7874=CARTESIAN_POINT('Origin',(7.25,2.,-2.2));
#7875=CARTESIAN_POINT('',(0.,0.,0.));
#7876=CARTESIAN_POINT('Origin',(-1.13137084989848,-1.13137084989848,6.7));
#7877=CARTESIAN_POINT('',(-1.29637084989848,-1.13137084989848,6.7));
#7878=CARTESIAN_POINT('Origin',(-1.13137084989848,-1.13137084989848,6.7));
#7879=CARTESIAN_POINT('',(-1.29637084989848,-1.13137084989848,8.));
#7880=CARTESIAN_POINT('',(-1.29637084989848,-1.13137084989848,6.7));
#7881=CARTESIAN_POINT('Origin',(-1.13137084989848,-1.13137084989848,8.));
#7882=CARTESIAN_POINT('Origin',(-1.13137084989848,-1.13137084989848,6.7));
#7883=CARTESIAN_POINT('Origin',(-1.13137084989848,1.13137084989848,6.7));
#7884=CARTESIAN_POINT('',(-1.29637084989848,1.13137084989848,6.7));
#7885=CARTESIAN_POINT('Origin',(-1.13137084989848,1.13137084989848,6.7));
#7886=CARTESIAN_POINT('',(-1.29637084989848,1.13137084989848,8.));
#7887=CARTESIAN_POINT('',(-1.29637084989848,1.13137084989848,6.7));
#7888=CARTESIAN_POINT('Origin',(-1.13137084989848,1.13137084989848,8.));
#7889=CARTESIAN_POINT('Origin',(-1.13137084989848,1.13137084989848,6.7));
#7890=CARTESIAN_POINT('Origin',(1.13137084989848,1.13137084989848,6.7));
#7891=CARTESIAN_POINT('',(0.966370849898476,1.13137084989848,6.7));
#7892=CARTESIAN_POINT('Origin',(1.13137084989848,1.13137084989848,6.7));
#7893=CARTESIAN_POINT('',(0.966370849898476,1.13137084989848,8.));
#7894=CARTESIAN_POINT('',(0.966370849898476,1.13137084989848,6.7));
#7895=CARTESIAN_POINT('Origin',(1.13137084989848,1.13137084989848,8.));
#7896=CARTESIAN_POINT('Origin',(1.13137084989848,1.13137084989848,6.7));
#7897=CARTESIAN_POINT('Origin',(1.13137084989848,-1.13137084989848,6.7));
#7898=CARTESIAN_POINT('',(0.966370849898476,-1.13137084989848,6.7));
#7899=CARTESIAN_POINT('Origin',(1.13137084989848,-1.13137084989848,6.7));
#7900=CARTESIAN_POINT('',(0.966370849898476,-1.13137084989848,8.));
#7901=CARTESIAN_POINT('',(0.966370849898476,-1.13137084989848,6.7));
#7902=CARTESIAN_POINT('Origin',(1.13137084989848,-1.13137084989848,8.));
#7903=CARTESIAN_POINT('Origin',(1.13137084989848,-1.13137084989848,6.7));
#7904=CARTESIAN_POINT('Origin',(1.2,-1.2,-0.1));
#7905=CARTESIAN_POINT('',(0.99,-1.2,0.));
#7906=CARTESIAN_POINT('Origin',(1.2,-1.2,0.));
#7907=CARTESIAN_POINT('',(0.99,-1.2,1.1));
#7908=CARTESIAN_POINT('',(0.99,-1.2,-0.1));
#7909=CARTESIAN_POINT('Origin',(1.2,-1.2,1.1));
#7910=CARTESIAN_POINT('Origin',(1.2,-1.2,1.1));
#7911=CARTESIAN_POINT('Origin',(-1.2,1.2,-0.1));
#7912=CARTESIAN_POINT('',(-1.41,1.2,0.));
#7913=CARTESIAN_POINT('Origin',(-1.2,1.2,0.));
#7914=CARTESIAN_POINT('',(-1.41,1.2,1.1));
#7915=CARTESIAN_POINT('',(-1.41,1.2,-0.1));
#7916=CARTESIAN_POINT('Origin',(-1.2,1.2,1.1));
#7917=CARTESIAN_POINT('Origin',(-1.2,1.2,1.1));
#7918=CARTESIAN_POINT('Origin',(-1.2,-1.2,-0.1));
#7919=CARTESIAN_POINT('',(-1.41,-1.2,0.));
#7920=CARTESIAN_POINT('Origin',(-1.2,-1.2,0.));
#7921=CARTESIAN_POINT('',(-1.41,-1.2,1.1));
#7922=CARTESIAN_POINT('',(-1.41,-1.2,-0.1));
#7923=CARTESIAN_POINT('Origin',(-1.2,-1.2,1.1));
#7924=CARTESIAN_POINT('Origin',(-1.2,-1.2,1.1));
#7925=CARTESIAN_POINT('Origin',(1.2,1.2,-0.1));
#7926=CARTESIAN_POINT('',(0.99,1.2,0.));
#7927=CARTESIAN_POINT('Origin',(1.2,1.2,0.));
#7928=CARTESIAN_POINT('',(0.99,1.2,1.1));
#7929=CARTESIAN_POINT('',(0.99,1.2,-0.1));
#7930=CARTESIAN_POINT('Origin',(1.2,1.2,1.1));
#7931=CARTESIAN_POINT('Origin',(1.2,1.2,1.1));
#7932=CARTESIAN_POINT('Origin',(0.,0.,3.5));
#7933=CARTESIAN_POINT('',(-1.05,-1.28587913910472E-16,3.5));
#7934=CARTESIAN_POINT('Origin',(0.,0.,3.5));
#7935=CARTESIAN_POINT('',(-1.05,1.28587913910472E-16,8.));
#7936=CARTESIAN_POINT('',(-1.05,-1.28587913910472E-16,3.5));
#7937=CARTESIAN_POINT('Origin',(0.,0.,8.));
#7938=CARTESIAN_POINT('Origin',(0.,0.,3.5));
#7939=CARTESIAN_POINT('',(-0.625,-7.65404249467096E-17,3.5));
#7940=CARTESIAN_POINT('Origin',(0.,0.,3.5));
#7941=CARTESIAN_POINT('Origin',(0.,0.,-0.1));
#7942=CARTESIAN_POINT('',(-0.625,-7.65404249467096E-17,0.));
#7943=CARTESIAN_POINT('Origin',(0.,0.,0.));
#7944=CARTESIAN_POINT('',(-0.625,-7.65404249467096E-17,-0.1));
#7945=CARTESIAN_POINT('Origin',(2.,2.,0.));
#7946=CARTESIAN_POINT('',(2.,2.,0.));
#7947=CARTESIAN_POINT('',(-2.,2.,0.));
#7948=CARTESIAN_POINT('',(2.,2.,0.));
#7949=CARTESIAN_POINT('',(-2.,2.,8.));
#7950=CARTESIAN_POINT('',(-2.,2.,0.));
#7951=CARTESIAN_POINT('',(2.,2.,8.));
#7952=CARTESIAN_POINT('',(2.,2.,8.));
#7953=CARTESIAN_POINT('',(2.,2.,0.));
#7954=CARTESIAN_POINT('Origin',(2.,-2.,0.));
#7955=CARTESIAN_POINT('',(2.,-2.,0.));
#7956=CARTESIAN_POINT('',(2.,-2.,0.));
#7957=CARTESIAN_POINT('',(2.,-2.,8.));
#7958=CARTESIAN_POINT('',(2.,-2.,8.));
#7959=CARTESIAN_POINT('',(2.,-2.,0.));
#7960=CARTESIAN_POINT('Origin',(-2.,-2.,0.));
#7961=CARTESIAN_POINT('',(-2.,-2.,0.));
#7962=CARTESIAN_POINT('',(-2.,-2.,0.));
#7963=CARTESIAN_POINT('',(-2.,-2.,8.));
#7964=CARTESIAN_POINT('',(-2.,-2.,8.));
#7965=CARTESIAN_POINT('',(-2.,-2.,0.));
#7966=CARTESIAN_POINT('Origin',(-2.,2.,0.));
#7967=CARTESIAN_POINT('',(-2.,2.,0.));
#7968=CARTESIAN_POINT('',(-2.,2.,8.));
#7969=CARTESIAN_POINT('Origin',(0.,0.,8.));
#7970=CARTESIAN_POINT('Origin',(0.,0.,0.));
#7971=CARTESIAN_POINT('',(0.,0.,0.));
#7972=CARTESIAN_POINT('Origin',(-1.13137084989848,-1.13137084989848,8.4));
#7973=CARTESIAN_POINT('',(-1.50637084989848,-1.13137084989848,8.4));
#7974=CARTESIAN_POINT('Origin',(-1.13137084989848,-1.13137084989848,8.4));
#7975=CARTESIAN_POINT('',(-1.50637084989848,-1.13137084989848,8.8));
#7976=CARTESIAN_POINT('',(-1.50637084989848,-1.13137084989848,8.4));
#7977=CARTESIAN_POINT('Origin',(-1.13137084989848,-1.13137084989848,8.8));
#7978=CARTESIAN_POINT('Origin',(-1.13137084989848,-1.13137084989848,8.4));
#7979=CARTESIAN_POINT('',(-1.35637084989848,-1.13137084989848,8.4));
#7980=CARTESIAN_POINT('Origin',(-1.13137084989848,-1.13137084989848,8.4));
#7981=CARTESIAN_POINT('Origin',(-1.13137084989848,1.13137084989848,8.4));
#7982=CARTESIAN_POINT('',(-1.50637084989848,1.13137084989848,8.4));
#7983=CARTESIAN_POINT('Origin',(-1.13137084989848,1.13137084989848,8.4));
#7984=CARTESIAN_POINT('',(-1.50637084989848,1.13137084989848,8.8));
#7985=CARTESIAN_POINT('',(-1.50637084989848,1.13137084989848,8.4));
#7986=CARTESIAN_POINT('Origin',(-1.13137084989848,1.13137084989848,8.8));
#7987=CARTESIAN_POINT('Origin',(-1.13137084989848,1.13137084989848,8.4));
#7988=CARTESIAN_POINT('',(-1.35637084989848,1.13137084989848,8.4));
#7989=CARTESIAN_POINT('Origin',(-1.13137084989848,1.13137084989848,8.4));
#7990=CARTESIAN_POINT('Origin',(1.13137084989848,1.13137084989848,8.4));
#7991=CARTESIAN_POINT('',(0.756370849898476,1.13137084989848,8.4));
#7992=CARTESIAN_POINT('Origin',(1.13137084989848,1.13137084989848,8.4));
#7993=CARTESIAN_POINT('',(0.756370849898476,1.13137084989848,8.8));
#7994=CARTESIAN_POINT('',(0.756370849898476,1.13137084989848,8.4));
#7995=CARTESIAN_POINT('Origin',(1.13137084989848,1.13137084989848,8.8));
#7996=CARTESIAN_POINT('Origin',(1.13137084989848,1.13137084989848,8.4));
#7997=CARTESIAN_POINT('',(0.906370849898476,1.13137084989848,8.4));
#7998=CARTESIAN_POINT('Origin',(1.13137084989848,1.13137084989848,8.4));
#7999=CARTESIAN_POINT('Origin',(1.13137084989848,-1.13137084989848,8.4));
#8000=CARTESIAN_POINT('',(0.756370849898476,-1.13137084989848,8.4));
#8001=CARTESIAN_POINT('Origin',(1.13137084989848,-1.13137084989848,8.4));
#8002=CARTESIAN_POINT('',(0.756370849898476,-1.13137084989848,8.8));
#8003=CARTESIAN_POINT('',(0.756370849898476,-1.13137084989848,8.4));
#8004=CARTESIAN_POINT('Origin',(1.13137084989848,-1.13137084989848,8.8));
#8005=CARTESIAN_POINT('Origin',(1.13137084989848,-1.13137084989848,8.4));
#8006=CARTESIAN_POINT('',(0.906370849898476,-1.13137084989848,8.4));
#8007=CARTESIAN_POINT('Origin',(1.13137084989848,-1.13137084989848,8.4));
#8008=CARTESIAN_POINT('Origin',(-1.13137084989848,-1.13137084989848,7.9));
#8009=CARTESIAN_POINT('',(-1.35637084989848,-1.13137084989848,8.));
#8010=CARTESIAN_POINT('Origin',(-1.13137084989848,-1.13137084989848,8.));
#8011=CARTESIAN_POINT('',(-1.35637084989848,-1.13137084989848,7.9));
#8012=CARTESIAN_POINT('Origin',(-1.13137084989848,1.13137084989848,7.9));
#8013=CARTESIAN_POINT('',(-1.35637084989848,1.13137084989848,8.));
#8014=CARTESIAN_POINT('Origin',(-1.13137084989848,1.13137084989848,8.));
#8015=CARTESIAN_POINT('',(-1.35637084989848,1.13137084989848,7.9));
#8016=CARTESIAN_POINT('Origin',(1.13137084989848,1.13137084989848,7.9));
#8017=CARTESIAN_POINT('',(0.906370849898476,1.13137084989848,8.));
#8018=CARTESIAN_POINT('Origin',(1.13137084989848,1.13137084989848,8.));
#8019=CARTESIAN_POINT('',(0.906370849898476,1.13137084989848,7.9));
#8020=CARTESIAN_POINT('Origin',(1.13137084989848,-1.13137084989848,7.9));
#8021=CARTESIAN_POINT('',(0.906370849898476,-1.13137084989848,8.));
#8022=CARTESIAN_POINT('Origin',(1.13137084989848,-1.13137084989848,8.));
#8023=CARTESIAN_POINT('',(0.906370849898476,-1.13137084989848,7.9));
#8024=CARTESIAN_POINT('Origin',(0.,0.,6.5));
#8025=CARTESIAN_POINT('',(-1.04,-1.27363267111325E-16,8.));
#8026=CARTESIAN_POINT('Origin',(0.,0.,8.));
#8027=CARTESIAN_POINT('',(-1.04,-1.27363267111325E-16,6.5));
#8028=CARTESIAN_POINT('',(-1.04,-1.27363267111325E-16,6.5));
#8029=CARTESIAN_POINT('Origin',(0.,0.,6.5));
#8030=CARTESIAN_POINT('Origin',(0.,0.,6.5));
#8031=CARTESIAN_POINT('',(-0.625,-7.65404249467096E-17,6.5));
#8032=CARTESIAN_POINT('Origin',(0.,0.,6.5));
#8033=CARTESIAN_POINT('Origin',(0.,0.,8.));
#8034=CARTESIAN_POINT('',(-0.625,-7.65404249467096E-17,8.8));
#8035=CARTESIAN_POINT('Origin',(0.,0.,8.8));
#8036=CARTESIAN_POINT('',(-0.625,-7.65404249467096E-17,8.));
#8037=CARTESIAN_POINT('Origin',(0.,0.,8.));
#8038=CARTESIAN_POINT('',(-2.,-2.44929359829471E-16,8.8));
#8039=CARTESIAN_POINT('Origin',(0.,0.,8.8));
#8040=CARTESIAN_POINT('',(-2.,-2.44929359829471E-16,8.));
#8041=CARTESIAN_POINT('',(-2.,-2.44929359829471E-16,8.));
#8042=CARTESIAN_POINT('Origin',(0.,0.,8.));
#8043=CARTESIAN_POINT('Origin',(0.,0.,8.8));
#8044=CARTESIAN_POINT('Origin',(0.,0.,8.));
#8045=CARTESIAN_POINT('',(0.,0.,0.));
#8046=CARTESIAN_POINT('Origin',(0.,0.,8.8));
#8047=CARTESIAN_POINT('',(-0.625,-7.65404249467096E-17,10.));
#8048=CARTESIAN_POINT('Origin',(0.,0.,10.));
#8049=CARTESIAN_POINT('',(-0.625,-7.65404249467096E-17,8.8));
#8050=CARTESIAN_POINT('',(-0.625,-7.65404249467096E-17,8.8));
#8051=CARTESIAN_POINT('Origin',(0.,0.,8.8));
#8052=CARTESIAN_POINT('Origin',(0.,0.,8.8));
#8053=CARTESIAN_POINT('',(-0.8,-9.79717439317883E-17,10.));
#8054=CARTESIAN_POINT('Origin',(0.,0.,10.));
#8055=CARTESIAN_POINT('',(-0.8,-9.79717439317883E-17,8.8));
#8056=CARTESIAN_POINT('',(-0.8,-9.79717439317883E-17,8.8));
#8057=CARTESIAN_POINT('Origin',(0.,0.,8.8));
#8058=CARTESIAN_POINT('Origin',(0.,0.,10.));
#8059=CARTESIAN_POINT('Origin',(0.,0.,8.8));
#8060=CARTESIAN_POINT('',(0.,0.,0.));
#8061=CARTESIAN_POINT('Ctrl Pts',(0.999999342796208,0.0048712153097108,
8.80019806641107));
#8062=CARTESIAN_POINT('Ctrl Pts',(0.99996896462742,0.230035163961994,8.81853897995701));
#8063=CARTESIAN_POINT('Ctrl Pts',(0.843216945008081,0.678245689353448,8.85526000727444));
#8064=CARTESIAN_POINT('Ctrl Pts',(0.23714388778331,1.05999084182087,8.91053070559157));
#8065=CARTESIAN_POINT('Ctrl Pts',(-0.476746387578999,0.979670338171269,
8.96597705173729));
#8066=CARTESIAN_POINT('Ctrl Pts',(-0.98657616663209,0.470389879273211,9.0216024298575));
#8067=CARTESIAN_POINT('Ctrl Pts',(-1.06798165663575,-0.248000588468906,
9.07740270249169));
#8068=CARTESIAN_POINT('Ctrl Pts',(-0.682243081073035,-0.862304425765768,
9.1333764236107));
#8069=CARTESIAN_POINT('Ctrl Pts',(-0.196330490445415,-1.03251494397982,
9.17314484390509));
#8070=CARTESIAN_POINT('Ctrl Pts',(0.0904960552365201,-1.02015022040365,
9.19657718102618));
#8071=CARTESIAN_POINT('Ctrl Pts',(0.204441911777542,-1.00572651008441,9.20595357869542));
#8072=CARTESIAN_POINT('Ctrl Pts',(0.343951015893895,-0.96975630344906,9.21768054548145));
#8073=CARTESIAN_POINT('Ctrl Pts',(0.501773879908335,-0.899045416054097,
9.23176320323934));
#8074=CARTESIAN_POINT('Ctrl Pts',(0.768592409823833,-0.721243151610969,
9.2578611494339));
#8075=CARTESIAN_POINT('Ctrl Pts',(1.04382114359922,-0.318042243912805,9.29602676229045));
#8076=CARTESIAN_POINT('Ctrl Pts',(1.04456490155922,0.326294295864951,9.34634267499162));
#8077=CARTESIAN_POINT('Ctrl Pts',(0.711307557250243,0.815326125223123,9.39257751006242));
#8078=CARTESIAN_POINT('Ctrl Pts',(0.234442425347365,1.04427973165066,9.43469552996756));
#8079=CARTESIAN_POINT('Ctrl Pts',(-0.242097506080382,1.04460426316974,9.47266669612882));
#8080=CARTESIAN_POINT('Ctrl Pts',(-0.672296189994615,0.837312084419627,
9.51070107270169));
#8081=CARTESIAN_POINT('Ctrl Pts',(-0.970493141256397,0.463551157181226,
9.54879683116503));
#8082=CARTESIAN_POINT('Ctrl Pts',(-1.07723336834064,-0.00342794058422688,
9.58695206272228));
#8083=CARTESIAN_POINT('Ctrl Pts',(-0.988260429843343,-0.39307851175747,
9.61879599421848));
#8084=CARTESIAN_POINT('Ctrl Pts',(-0.82093539560644,-0.658946730224756,
9.64429884892662));
#8085=CARTESIAN_POINT('Ctrl Pts',(-0.598840710302034,-0.88141322392247,
9.66981982299092));
#8086=CARTESIAN_POINT('Ctrl Pts',(-0.237756057923814,-1.05547919442497,
9.70175433946707));
#8087=CARTESIAN_POINT('Ctrl Pts',(0.243905786180905,-1.05553040152794,9.74012683420727));
#8088=CARTESIAN_POINT('Ctrl Pts',(0.678604028637572,-0.846341399380819,
9.77854812145871));
#8089=CARTESIAN_POINT('Ctrl Pts',(0.979430107833126,-0.468912235308927,
9.81701586224876));
#8090=CARTESIAN_POINT('Ctrl Pts',(1.09985901046267,0.0548445677701001,9.85980673545165));
#8091=CARTESIAN_POINT('Ctrl Pts',(0.921933505746503,0.631124795915794,9.90693599171239));
#8092=CARTESIAN_POINT('Ctrl Pts',(0.4929126040201,0.973793160670524,9.94983738646297));
#8093=CARTESIAN_POINT('Ctrl Pts',(0.0780904371091028,1.06751269479759,9.98418939216924));
#8094=CARTESIAN_POINT('Ctrl Pts',(-0.346188348797786,1.0365452542535,10.0185609429505));
#8095=CARTESIAN_POINT('Ctrl Pts',(-0.822968443953264,0.76162232341949,10.0615600576428));
#8096=CARTESIAN_POINT('Ctrl Pts',(-1.11011929233597,0.166104281872854,10.1132080400722));
#8097=CARTESIAN_POINT('Ctrl Pts',(-1.0081246602054,-0.515708350877839,10.1670522944212));
#8098=CARTESIAN_POINT('Ctrl Pts',(-0.494775946618556,-1.02970801548153,
10.2230915794475));
#8099=CARTESIAN_POINT('Ctrl Pts',(0.171330015334639,-1.10394798748412,10.2748519542969));
#8100=CARTESIAN_POINT('Ctrl Pts',(0.683814393710209,-0.85633240678914,10.3201591760856));
#8101=CARTESIAN_POINT('Ctrl Pts',(0.987375224349673,-0.475369257557772,
10.3590026286433));
#8102=CARTESIAN_POINT('Ctrl Pts',(1.11501021817459,0.0796008030233853,10.4043267361272));
#8103=CARTESIAN_POINT('Ctrl Pts',(0.894257942603671,0.712772351603783,10.4561304980607));
#8104=CARTESIAN_POINT('Ctrl Pts',(0.254526418580225,1.11465334671006,10.5144063331842));
#8105=CARTESIAN_POINT('Ctrl Pts',(-0.495386650979013,1.03000796421648,10.5726689321936));
#8106=CARTESIAN_POINT('Ctrl Pts',(-1.02902006816757,0.496451864872819,10.6309084916996));
#8107=CARTESIAN_POINT('Ctrl Pts',(-1.11329107431628,-0.25302544687232,10.6891152782939));
#8108=CARTESIAN_POINT('Ctrl Pts',(-0.712411475504087,-0.890954531307481,
10.7472796615617));
#8109=CARTESIAN_POINT('Ctrl Pts',(-0.00144545535703713,-1.13970545531556,
10.8053921361455));
#8110=CARTESIAN_POINT('Ctrl Pts',(0.589562318042014,-0.932130645422847,
10.8537681412278));
#8111=CARTESIAN_POINT('Ctrl Pts',(0.908494555547074,-0.573322783618425,
10.8924337348326));
#8112=CARTESIAN_POINT('Ctrl Pts',(1.0932000203843,-0.130460109720627,10.9310743576345));
#8113=CARTESIAN_POINT('Ctrl Pts',(1.02452819258886,0.49024714203063,10.9793255246093));
#8114=CARTESIAN_POINT('Ctrl Pts',(0.493612168598575,1.02033558321459,11.037138824411));
#8115=CARTESIAN_POINT('Ctrl Pts',(-0.166230575259128,1.09368100121347,11.0884425957329));
#8116=CARTESIAN_POINT('Ctrl Pts',(-0.673140522140151,0.84850197959383,11.1332655331794));
#8117=CARTESIAN_POINT('Ctrl Pts',(-0.973483979429893,0.47222295927322,11.1716363210045));
#8118=CARTESIAN_POINT('Ctrl Pts',(-1.08028898641827,0.00311472479435195,
11.2099559586628));
#8119=CARTESIAN_POINT('Ctrl Pts',(-0.973354083483389,-0.465125791076451,
11.2482222395404));
#8120=CARTESIAN_POINT('Ctrl Pts',(-0.674252322492463,-0.840091585392608,
11.2864330284043));
#8121=CARTESIAN_POINT('Ctrl Pts',(-0.242715089956039,-1.04789098180051,
11.3245862592493));
#8122=CARTESIAN_POINT('Ctrl Pts',(0.23542767696283,-1.04765866302507,11.3626799542613));
#8123=CARTESIAN_POINT('Ctrl Pts',(0.665536159094464,-0.840435751119737,
11.4007121983223));
#8124=CARTESIAN_POINT('Ctrl Pts',(0.962591820228485,-0.467820172164233,
11.4386811727585));
#8125=CARTESIAN_POINT('Ctrl Pts',(1.06846208937938,-0.00379118886353965,
11.47658513569));
#8126=CARTESIAN_POINT('Ctrl Pts',(0.962501175338684,0.458913289962351,11.5144224357756));
#8127=CARTESIAN_POINT('Ctrl Pts',(0.618041205754224,0.892154566858533,11.5584863515166));
#8128=CARTESIAN_POINT('Ctrl Pts',(0.00421838652791971,1.10738146763147,
11.6087289304493));
#8129=CARTESIAN_POINT('Ctrl Pts',(-0.685284502455283,0.86560690604705,11.6650903417562));
#8130=CARTESIAN_POINT('Ctrl Pts',(-1.07219887432344,0.249028474249683,11.7212863124465));
#8131=CARTESIAN_POINT('Ctrl Pts',(-0.990640181337795,-0.472396051339649,
11.7773128627812));
#8132=CARTESIAN_POINT('Ctrl Pts',(-0.478640001005609,-0.983760746265736,
11.8331676524783));
#8133=CARTESIAN_POINT('Ctrl Pts',(0.238202676882345,-1.06445286799178,11.8888462567429));
#8134=CARTESIAN_POINT('Ctrl Pts',(0.846858663881909,-0.681098479204223,
11.9443505326692));
#8135=CARTESIAN_POINT('Ctrl Pts',(1.00427568511571,-0.230977292777482,11.9812290386622));
#8136=CARTESIAN_POINT('Ctrl Pts',(1.00430619197361,-0.004859230773597,11.9996476704237));
#8137=CARTESIAN_POINT('Ctrl Pts',(0.982047384939078,0.00486879330739147,
8.80019806641107));
#8138=CARTESIAN_POINT('Ctrl Pts',(0.982017542571237,0.226061368380877,8.8182154884749));
#8139=CARTESIAN_POINT('Ctrl Pts',(0.828073759479322,0.666265246409587,8.85427793870567));
#8140=CARTESIAN_POINT('Ctrl Pts',(0.232718051648345,1.04130280902705,8.90857206776144));
#8141=CARTESIAN_POINT('Ctrl Pts',(-0.468680551990921,0.962405317361456,
8.96304474127639));
#8142=CARTESIAN_POINT('Ctrl Pts',(-0.969725556632444,0.461952106094082,
9.01770706443454));
#8143=CARTESIAN_POINT('Ctrl Pts',(-1.04978892409544,-0.24421501980538,9.07255473573053));
#8144=CARTESIAN_POINT('Ctrl Pts',(-0.670526282680969,-0.848287475569065,
9.12759197393209));
#8145=CARTESIAN_POINT('Ctrl Pts',(-0.192569344974563,-1.01574821805213,
9.16670672447678));
#8146=CARTESIAN_POINT('Ctrl Pts',(0.0896475808341612,-1.00358230969371,
9.18976208492581));
#8147=CARTESIAN_POINT('Ctrl Pts',(0.201768534269143,-0.989389860609658,
9.19898826062923));
#8148=CARTESIAN_POINT('Ctrl Pts',(0.339053092327797,-0.953994606992962,
9.21052787927458));
#8149=CARTESIAN_POINT('Ctrl Pts',(0.494377601147851,-0.884404812313703,
9.22438724394839));
#8150=CARTESIAN_POINT('Ctrl Pts',(0.757001856405022,-0.709402012144092,
9.25007419376896));
#8151=CARTESIAN_POINT('Ctrl Pts',(1.0279911029959,-0.312481730693998,9.28764301092837));
#8152=CARTESIAN_POINT('Ctrl Pts',(1.02877459893023,0.322165970926696,9.33720097094436));
#8153=CARTESIAN_POINT('Ctrl Pts',(0.700413157880328,0.804092297036147,9.38275776600637));
#8154=CARTESIAN_POINT('Ctrl Pts',(0.230301769583314,1.02983016988876,9.42427724831843));
#8155=CARTESIAN_POINT('Ctrl Pts',(-0.239683635592506,1.03017515445717,9.46172242153018));
#8156=CARTESIAN_POINT('Ctrl Pts',(-0.664163045312016,0.825661502108212,
9.49924891917935));
#8157=CARTESIAN_POINT('Ctrl Pts',(-0.958529939902563,0.456745656141783,
9.53684906905032));
#8158=CARTESIAN_POINT('Ctrl Pts',(-1.06396267414552,-0.00440524776029272,
9.5745255639511));
#8159=CARTESIAN_POINT('Ctrl Pts',(-0.976079979910487,-0.389373735213914,
9.60598297021468));
#8160=CARTESIAN_POINT('Ctrl Pts',(-0.810705582541046,-0.652150929778934,
9.63118793351945));
#8161=CARTESIAN_POINT('Ctrl Pts',(-0.591146716083035,-0.872084267774335,
9.6564168813747));
#8162=CARTESIAN_POINT('Ctrl Pts',(-0.234072078906085,-1.04424533055482,
9.68799397302578));
#8163=CARTESIAN_POINT('Ctrl Pts',(0.242500469223428,-1.04432630242473,9.72595785040098));
#8164=CARTESIAN_POINT('Ctrl Pts',(0.672838065087217,-0.83726980079961,9.7639884443319));
#8165=CARTESIAN_POINT('Ctrl Pts',(0.970815428000762,-0.463458065904377,
9.80208605881035));
#8166=CARTESIAN_POINT('Ctrl Pts',(1.09019540146654,0.0555635056652221,9.84448580287717));
#8167=CARTESIAN_POINT('Ctrl Pts',(0.913813691461406,0.627036825844031,9.89121709087636));
#8168=CARTESIAN_POINT('Ctrl Pts',(0.48811414653708,0.967138669436487,9.93378708715817));
#8169=CARTESIAN_POINT('Ctrl Pts',(0.0762229670049308,1.06020598638962,9.96789328622913));
#8170=CARTESIAN_POINT('Ctrl Pts',(-0.345222042701214,1.0294593023382,10.0020337480872));
#8171=CARTESIAN_POINT('Ctrl Pts',(-0.819095169387929,0.756280403334857,
10.044760955629));
#8172=CARTESIAN_POINT('Ctrl Pts',(-1.10479169712882,0.163970602181336,10.0961315732279));
#8173=CARTESIAN_POINT('Ctrl Pts',(-1.00334187935937,-0.514754332116599,
10.1497258011113));
#8174=CARTESIAN_POINT('Ctrl Pts',(-0.491985150485256,-1.0269135369247,10.2055489936168));
#8175=CARTESIAN_POINT('Ctrl Pts',(0.172230476805367,-1.10104324987106,10.2571555969155));
#8176=CARTESIAN_POINT('Ctrl Pts',(0.6837034079542,-0.853959036612514,10.3023689497361));
#8177=CARTESIAN_POINT('Ctrl Pts',(0.986863059949987,-0.473547176850352,
10.3411560919635));
#8178=CARTESIAN_POINT('Ctrl Pts',(1.11443827396583,0.0809655868366956,10.3864406203787));
#8179=CARTESIAN_POINT('Ctrl Pts',(0.893794220249733,0.714129022372665,10.4382345485064));
#8180=CARTESIAN_POINT('Ctrl Pts',(0.253564991089117,1.11646188695564,10.4965555791176));
#8181=CARTESIAN_POINT('Ctrl Pts',(-0.497710807257122,1.03177486246381,10.5549164707911));
#8182=CARTESIAN_POINT('Ctrl Pts',(-1.03287455412715,0.496850894811073,10.6133080838302));
#8183=CARTESIAN_POINT('Ctrl Pts',(-1.11756500239139,-0.255330318551581,
10.6717198630721));
#8184=CARTESIAN_POINT('Ctrl Pts',(-0.714971732167115,-0.896204048773918,
10.7301410140639));
#8185=CARTESIAN_POINT('Ctrl Pts',(-0.000197744427673544,-1.14640555699347,
10.7885625557949));
#8186=CARTESIAN_POINT('Ctrl Pts',(0.594542321544182,-0.937612040665249,
10.8372358480802));
#8187=CARTESIAN_POINT('Ctrl Pts',(0.915705377171634,-0.576320258708504,
10.8761680572913));
#8188=CARTESIAN_POINT('Ctrl Pts',(1.10178414791373,-0.130204417591924,10.915091761851));
#8189=CARTESIAN_POINT('Ctrl Pts',(1.03265373134923,0.495463186235901,10.9637246794375));
#8190=CARTESIAN_POINT('Ctrl Pts',(0.497145233405868,1.03028230225543,11.0220401925551));
#8191=CARTESIAN_POINT('Ctrl Pts',(-0.169012977210461,1.10441503835764,11.0738304261316));
#8192=CARTESIAN_POINT('Ctrl Pts',(-0.681133539914993,0.85674905407542,11.1191103749823));
#8193=CARTESIAN_POINT('Ctrl Pts',(-0.984721103773031,0.476446874844114,
11.1578900621551));
#8194=CARTESIAN_POINT('Ctrl Pts',(-1.092751156294,0.00206620542347027,11.1966396932756));
#8195=CARTESIAN_POINT('Ctrl Pts',(-0.98459016094734,-0.471660870020862,
11.2353514494943));
#8196=CARTESIAN_POINT('Ctrl Pts',(-0.681864802424284,-0.851204764218623,
11.2740254978417));
#8197=CARTESIAN_POINT('Ctrl Pts',(-0.244894669388729,-1.06164493769735,
11.3126574520722));
#8198=CARTESIAN_POINT('Ctrl Pts',(0.239497914027533,-1.06142946990311,11.3512480535563));
#8199=CARTESIAN_POINT('Ctrl Pts',(0.675410001418759,-0.85143262563631,11.3897909190191));
#8200=CARTESIAN_POINT('Ctrl Pts',(0.97660256231849,-0.47365645262325,11.4282852412925));
#8201=CARTESIAN_POINT('Ctrl Pts',(1.08400003731686,-0.00301072745489087,
11.4667285195545));
#8202=CARTESIAN_POINT('Ctrl Pts',(0.976502876676812,0.466470502386992,11.5051182694331));
#8203=CARTESIAN_POINT('Ctrl Pts',(0.626894863562504,0.906218485725883,11.549841630365));
#8204=CARTESIAN_POINT('Ctrl Pts',(0.00363437595233928,1.12480301808217,
11.600855774006));
#8205=CARTESIAN_POINT('Ctrl Pts',(-0.696824177011358,0.879241198259212,
11.6581097453269));
#8206=CARTESIAN_POINT('Ctrl Pts',(-1.09007389999346,0.25264708501371,11.7152189643452));
#8207=CARTESIAN_POINT('Ctrl Pts',(-1.00719470908938,-0.480789320374471,
11.7721773844949));
#8208=CARTESIAN_POINT('Ctrl Pts',(-0.486528264941766,-1.00085757657432,
11.8289789551926));
#8209=CARTESIAN_POINT('Ctrl Pts',(0.242674951053419,-1.08295512724231,11.8856179806837));
#8210=CARTESIAN_POINT('Ctrl Pts',(0.861972926357441,-0.692938107583723,
11.9420899351664));
#8211=CARTESIAN_POINT('Ctrl Pts',(1.02218081422145,-0.234837326490113,11.9796219395556));
#8212=CARTESIAN_POINT('Ctrl Pts',(1.02221185564686,-0.00475702858911594,
11.9983633184843));
#8213=CARTESIAN_POINT('Ctrl Pts',(0.946251939821601,0.00346790923095878,
8.81733686319961));
#8214=CARTESIAN_POINT('Ctrl Pts',(0.946223170149248,0.216709631387298,8.83470664203795));
#8215=CARTESIAN_POINT('Ctrl Pts',(0.797868558912845,0.640717122048251,8.86944390364538));
#8216=CARTESIAN_POINT('Ctrl Pts',(0.224685675994098,1.00171482448492,8.92171403423268));
#8217=CARTESIAN_POINT('Ctrl Pts',(-0.450094354194183,0.925721174112207,
8.97411924922092));
#8218=CARTESIAN_POINT('Ctrl Pts',(-0.931851520616104,0.444457369493084,
9.02668243919957));
#8219=CARTESIAN_POINT('Ctrl Pts',(-1.00876374936087,-0.234332975359601,
9.07940345376113));
#8220=CARTESIAN_POINT('Ctrl Pts',(-0.644280498352913,-0.814814073429451,
9.132293292668));
#8221=CARTESIAN_POINT('Ctrl Pts',(-0.185030806522485,-0.975710075967432,
9.16987780176979));
#8222=CARTESIAN_POINT('Ctrl Pts',(0.0861306964382634,-0.964020787510786,
9.19203012360292));
#8223=CARTESIAN_POINT('Ctrl Pts',(0.193859203693136,-0.950384199462588,
9.20089488110907));
#8224=CARTESIAN_POINT('Ctrl Pts',(0.325766432724325,-0.916374835785051,
9.21198266561942));
#8225=CARTESIAN_POINT('Ctrl Pts',(0.475008489408351,-0.849509651707339,
9.22529946397773));
#8226=CARTESIAN_POINT('Ctrl Pts',(0.72735253136785,-0.681355419969213,9.2499813528838));
#8227=CARTESIAN_POINT('Ctrl Pts',(0.987759532431315,-0.299937694770344,
9.28608546277695));
#8228=CARTESIAN_POINT('Ctrl Pts',(0.988529254394412,0.31002344397511,9.33371680705976));
#8229=CARTESIAN_POINT('Ctrl Pts',(0.67286673528341,0.773354286803788,9.37751699303838));
#8230=CARTESIAN_POINT('Ctrl Pts',(0.220764282478621,0.990462726141864,9.41744839941452));
#8231=CARTESIAN_POINT('Ctrl Pts',(-0.23137446087799,0.990807495240239,9.45347433529735));
#8232=CARTESIAN_POINT('Ctrl Pts',(-0.639893401702073,0.794007818769354,
9.48958994897445));
#8233=CARTESIAN_POINT('Ctrl Pts',(-0.923327263108843,0.438822435846309,
9.52579447470907));
#8234=CARTESIAN_POINT('Ctrl Pts',(-1.02491137571836,-0.00538407263128216,
9.56208933392858));
#8235=CARTESIAN_POINT('Ctrl Pts',(-0.940232267608687,-0.376417877351174,
9.59241037531266));
#8236=CARTESIAN_POINT('Ctrl Pts',(-0.780786057662726,-0.629783667326523,
9.61671320097693));
#8237=CARTESIAN_POINT('Ctrl Pts',(-0.569033793255791,-0.841902767826415,
9.64104641368153));
#8238=CARTESIAN_POINT('Ctrl Pts',(-0.224489149210013,-1.0080482857871,9.67151952337384));
#8239=CARTESIAN_POINT('Ctrl Pts',(0.235673510791263,-1.00815805640934,9.70817893472068));
#8240=CARTESIAN_POINT('Ctrl Pts',(0.651503567024935,-0.808120949371662,
9.74492970282906));
#8241=CARTESIAN_POINT('Ctrl Pts',(0.939670159494493,-0.446677535335527,
9.78177187806484));
#8242=CARTESIAN_POINT('Ctrl Pts',(1.05523972468657,0.0555890051172364,9.82280879182749));
#8243=CARTESIAN_POINT('Ctrl Pts',(0.884483903066246,0.609188073050605,9.86807884630888));
#8244=CARTESIAN_POINT('Ctrl Pts',(0.471693669376953,0.939087262360839,9.90936701071719));
#8245=CARTESIAN_POINT('Ctrl Pts',(0.0718701946233878,1.02945078127861,9.94247676831493));
#8246=CARTESIAN_POINT('Ctrl Pts',(-0.337475699762535,0.999603452125411,
9.97563909649433));
#8247=CARTESIAN_POINT('Ctrl Pts',(-0.798276925818471,0.734084817620259,
10.0171900420759));
#8248=CARTESIAN_POINT('Ctrl Pts',(-1.0765334634925,0.157487645860965,10.0672053034725));
#8249=CARTESIAN_POINT('Ctrl Pts',(-0.977769536461385,-0.504250043799724,
10.1194626321329));
#8250=CARTESIAN_POINT('Ctrl Pts',(-0.478575291848728,-1.00451835916292,
10.1739816819444));
#8251=CARTESIAN_POINT('Ctrl Pts',(0.171126569807208,-1.07721754138009,10.2244700816925));
#8252=CARTESIAN_POINT('Ctrl Pts',(0.672182788674072,-0.835256219302107,
10.2687619732111));
#8253=CARTESIAN_POINT('Ctrl Pts',(0.969547810320499,-0.462213248235356,
10.3068036909456));
#8254=CARTESIAN_POINT('Ctrl Pts',(1.09489348151214,0.0822563931149444,10.3512740281145));
#8255=CARTESIAN_POINT('Ctrl Pts',(0.878086601000876,0.705028239333339,10.4022206349257));
#8256=CARTESIAN_POINT('Ctrl Pts',(0.247376731962901,1.10167051144662,10.4596936844876));
#8257=CARTESIAN_POINT('Ctrl Pts',(-0.494343825650103,1.01831274777828,10.5173179494214));
#8258=CARTESIAN_POINT('Ctrl Pts',(-1.02389367392556,0.489356402466505,10.5750854103097));
#8259=CARTESIAN_POINT('Ctrl Pts',(-1.1080879323535,-0.256139394666961,10.6329877640774));
#8260=CARTESIAN_POINT('Ctrl Pts',(-0.708467620348485,-0.892752715736136,
10.6910165384584));
#8261=CARTESIAN_POINT('Ctrl Pts',(0.00275806339120792,-1.14199252167361,
10.7491621240617));
#8262=CARTESIAN_POINT('Ctrl Pts',(0.595915072591307,-0.933982364866608,
10.7977073894074));
#8263=CARTESIAN_POINT('Ctrl Pts',(0.916693997947134,-0.573186172446775,
10.8365910184109));
#8264=CARTESIAN_POINT('Ctrl Pts',(1.10275571560074,-0.127229568265828,10.8755054547366));
#8265=CARTESIAN_POINT('Ctrl Pts',(1.03374107847987,0.499230126741185,10.9242044521008));
#8266=CARTESIAN_POINT('Ctrl Pts',(0.496651096330989,1.03602339561547,10.982721896355));
#8267=CARTESIAN_POINT('Ctrl Pts',(-0.173057151953294,1.11077134701646,11.0347972056812));
#8268=CARTESIAN_POINT('Ctrl Pts',(-0.688810280773869,0.861454433490338,
11.0803977479046));
#8269=CARTESIAN_POINT('Ctrl Pts',(-0.994990321540318,0.478015999913525,
11.1195067251792));
#8270=CARTESIAN_POINT('Ctrl Pts',(-1.10413900699883,-0.000930907827253689,
11.1586323799395));
#8271=CARTESIAN_POINT('Ctrl Pts',(-0.994852434030972,-0.479892724154501,
11.1977747838273));
#8272=CARTESIAN_POINT('Ctrl Pts',(-0.688454851688791,-0.864158828181502,
11.2369285531699));
#8273=CARTESIAN_POINT('Ctrl Pts',(-0.245556936433115,-1.07753293814173,
11.2760917573129));
#8274=CARTESIAN_POINT('Ctrl Pts',(0.246044401600366,-1.0773877681717,11.3152583014517));
#8275=CARTESIAN_POINT('Ctrl Pts',(0.689038817571119,-0.864056889518542,
11.3544280678403));
#8276=CARTESIAN_POINT('Ctrl Pts',(0.995533503363568,-0.479743995432174,
11.3935962007367));
#8277=CARTESIAN_POINT('Ctrl Pts',(1.10500493611492,-0.000336441793609564,
11.432759423983));
#8278=CARTESIAN_POINT('Ctrl Pts',(0.995437508199075,0.478484225555593,11.471914533027));
#8279=CARTESIAN_POINT('Ctrl Pts',(0.638543403370204,0.927530552036555,11.5175815981191));
#8280=CARTESIAN_POINT('Ctrl Pts',(0.00131834384992748,1.1512205599446,11.5697498749575));
#8281=CARTESIAN_POINT('Ctrl Pts',(-0.716162033397229,0.899924142153474,
11.6283938640621));
#8282=CARTESIAN_POINT('Ctrl Pts',(-1.11974363778359,0.257254170951805,11.6869825988179));
#8283=CARTESIAN_POINT('Ctrl Pts',(-1.03478697806096,-0.496287761111256,
11.7455056502723));
#8284=CARTESIAN_POINT('Ctrl Pts',(-0.499211397844794,-1.0315157806068,11.8039508889109));
#8285=CARTESIAN_POINT('Ctrl Pts',(0.25207649193241,-1.11624858861966,11.8623120440781));
#8286=CARTESIAN_POINT('Ctrl Pts',(0.891057567372483,-0.71406944827229,11.9205699244295));
#8287=CARTESIAN_POINT('Ctrl Pts',(1.05664899061948,-0.24083687143616,11.9593476619553));
#8288=CARTESIAN_POINT('Ctrl Pts',(1.05668105685756,-0.00316062068079096,
11.9787077754391));
#8289=CARTESIAN_POINT('Ctrl Pts',(0.933110845774544,-0.00124761587970791,
8.87520568466563));
#8290=CARTESIAN_POINT('Ctrl Pts',(0.933082485311987,0.208961030315505,8.89232840182152));
#8291=CARTESIAN_POINT('Ctrl Pts',(0.786770179169481,0.626345163412827,8.92653493659135));
#8292=CARTESIAN_POINT('Ctrl Pts',(0.224133602875593,0.980245228608542,8.97782692366071));
#8293=CARTESIAN_POINT('Ctrl Pts',(-0.435812671372105,0.905573247736591,
9.02908909375654));
#8294=CARTESIAN_POINT('Ctrl Pts',(-0.905278949446739,0.436102668627462,
9.08034196302577));
#8295=CARTESIAN_POINT('Ctrl Pts',(-0.979701853601785,-0.223724459540056,
9.13159318793611));
#8296=CARTESIAN_POINT('Ctrl Pts',(-0.626199332431556,-0.786111248844846,
9.18285439354528));
#8297=CARTESIAN_POINT('Ctrl Pts',(-0.182309307756624,-0.941401852206475,
9.21918157669349));
#8298=CARTESIAN_POINT('Ctrl Pts',(0.0793196104033138,-0.930122621318997,
9.24055595057928));
#8299=CARTESIAN_POINT('Ctrl Pts',(0.183226682424838,-0.916969037284389,
9.24910628913725));
#8300=CARTESIAN_POINT('Ctrl Pts',(0.310391085781095,-0.884178026616486,
9.25979589713383));
#8301=CARTESIAN_POINT('Ctrl Pts',(0.454169054244644,-0.819756142740368,
9.27262568518493));
#8302=CARTESIAN_POINT('Ctrl Pts',(0.697116053142912,-0.657850695056992,
9.29638934987471));
#8303=CARTESIAN_POINT('Ctrl Pts',(0.947351969011777,-0.291063703435681,
9.33110485588488));
#8304=CARTESIAN_POINT('Ctrl Pts',(0.947893979854482,0.294038239775498,9.37679585569485));
#8305=CARTESIAN_POINT('Ctrl Pts',(0.64559614597452,0.737470402080906,9.41872694647258));
#8306=CARTESIAN_POINT('Ctrl Pts',(0.213542771693588,0.944865687214638,9.456887453317));
#8307=CARTESIAN_POINT('Ctrl Pts',(-0.21790942255983,0.945130416632738,9.49126781446859));
#8308=CARTESIAN_POINT('Ctrl Pts',(-0.607175295083612,0.757538118255783,
9.52568490650978));
#8309=CARTESIAN_POINT('Ctrl Pts',(-0.876886139203015,0.419454940311435,
9.5601447217719));
#8310=CARTESIAN_POINT('Ctrl Pts',(-0.973399204055829,-0.00281983355499825,
9.59464850829951));
#8311=CARTESIAN_POINT('Ctrl Pts',(-0.892953621384232,-0.355121345095021,
9.62344157007163));
#8312=CARTESIAN_POINT('Ctrl Pts',(-0.741670531971874,-0.595502068510008,
9.64649995731916));
#8313=CARTESIAN_POINT('Ctrl Pts',(-0.540861334347598,-0.79664831552706,
9.66957548515654));
#8314=CARTESIAN_POINT('Ctrl Pts',(-0.214347909139945,-0.954058224911974,
9.69845416164799));
#8315=CARTESIAN_POINT('Ctrl Pts',(0.221317761541613,-0.954121235060302,
9.73316338989386));
#8316=CARTESIAN_POINT('Ctrl Pts',(0.614674372570484,-0.764854624133257,
9.76793103575109));
#8317=CARTESIAN_POINT('Ctrl Pts',(0.887052993147029,-0.423164929085746,
9.80275900129157));
#8318=CARTESIAN_POINT('Ctrl Pts',(0.996196176963173,0.0513246907769201,
9.8415273466477));
#8319=CARTESIAN_POINT('Ctrl Pts',(0.834948113879409,0.573926065074171,9.88426514494727));
#8320=CARTESIAN_POINT('Ctrl Pts',(0.44547575217633,0.885137394010584,9.92321920683063));
#8321=CARTESIAN_POINT('Ctrl Pts',(0.0684014908627373,0.970356094387837,
9.95444592358018));
#8322=CARTESIAN_POINT('Ctrl Pts',(-0.317575790754665,0.942207118119873,
9.98571530594194));
#8323=CARTESIAN_POINT('Ctrl Pts',(-0.751956369176069,0.691895051315754,
10.0248858146619));
#8324=CARTESIAN_POINT('Ctrl Pts',(-1.01420012669963,0.148454419987656,10.0720248209112));
#8325=CARTESIAN_POINT('Ctrl Pts',(-0.921125606711717,-0.475192219958838,
10.1212746978924));
#8326=CARTESIAN_POINT('Ctrl Pts',(-0.450640791192364,-0.946727050507445,
10.1726608327701));
#8327=CARTESIAN_POINT('Ctrl Pts',(0.161885358038663,-1.0153085919114,10.2202607279042));
#8328=CARTESIAN_POINT('Ctrl Pts',(0.634464325836929,-0.7871254203658,10.2620342877094));
#8329=CARTESIAN_POINT('Ctrl Pts',(0.915044949089008,-0.435171331085412,
10.2979265084477));
#8330=CARTESIAN_POINT('Ctrl Pts',(1.0333921730293,0.0787559345129345,10.3399027505605));
#8331=CARTESIAN_POINT('Ctrl Pts',(0.828697304223945,0.667017539209564,10.3880228606081));
#8332=CARTESIAN_POINT('Ctrl Pts',(0.232467374207285,1.04212743993356,10.4423591262489));
#8333=CARTESIAN_POINT('Ctrl Pts',(-0.469582947467488,0.963374254330498,
10.4968986206485));
#8334=CARTESIAN_POINT('Ctrl Pts',(-0.971549690422633,0.462203568299623,
10.5516426651414));
#8335=CARTESIAN_POINT('Ctrl Pts',(-1.05163594424887,-0.245277711367363,
10.6065920927203));
#8336=CARTESIAN_POINT('Ctrl Pts',(-0.671962136426674,-0.850494803107478,
10.6617469196619));
#8337=CARTESIAN_POINT('Ctrl Pts',(0.00514473529517556,-1.08801203030429,
10.7171069354582));
#8338=CARTESIAN_POINT('Ctrl Pts',(0.571006381985689,-0.889777195779423,
10.7634098332665));
#8339=CARTESIAN_POINT('Ctrl Pts',(0.877482655626295,-0.545130724676744,
10.8005540126445));
#8340=CARTESIAN_POINT('Ctrl Pts',(1.05543893274011,-0.118705473665279,10.8377653530311));
#8341=CARTESIAN_POINT('Ctrl Pts',(0.989557126951709,0.481292167662269,10.8844038712234));
#8342=CARTESIAN_POINT('Ctrl Pts',(0.474249124300982,0.996731925119642,10.9405665516539));
#8343=CARTESIAN_POINT('Ctrl Pts',(-0.170018784224988,1.06889843758203,10.9906607188205));
#8344=CARTESIAN_POINT('Ctrl Pts',(-0.667252349418254,0.828652140244528,
11.0346171254776));
#8345=CARTESIAN_POINT('Ctrl Pts',(-0.962957118749545,0.458476875796659,
11.0723761453514));
#8346=CARTESIAN_POINT('Ctrl Pts',(-1.06861617984619,-0.00474659541608284,
11.1102178529854));
#8347=CARTESIAN_POINT('Ctrl Pts',(-0.962829285747689,-0.468812774742328,
11.1481382421668));
#8348=CARTESIAN_POINT('Ctrl Pts',(-0.66552637265583,-0.841826091853817,
11.1861371971565));
#8349=CARTESIAN_POINT('Ctrl Pts',(-0.234945846970159,-1.0493782184629,11.2242118409212));
#8350=CARTESIAN_POINT('Ctrl Pts',(0.243922228184406,-1.04933364959166,11.2623624755123));
#8351=CARTESIAN_POINT('Ctrl Pts',(0.676275279337915,-0.841241205435662,
11.3005845553303));
#8352=CARTESIAN_POINT('Ctrl Pts',(0.976019367363091,-0.465554703444286,
11.3388772265428));
#8353=CARTESIAN_POINT('Ctrl Pts',(1.08335811630658,0.00404254183906937,
11.3772382701768));
#8354=CARTESIAN_POINT('Ctrl Pts',(0.975916530883124,0.474019295230167,11.4156652984567));
#8355=CARTESIAN_POINT('Ctrl Pts',(0.625055282289429,0.915683137019696,11.4605716003999));
#8356=CARTESIAN_POINT('Ctrl Pts',(-0.00300719915789507,1.13650050171769,
11.5119933522144));
#8357=CARTESIAN_POINT('Ctrl Pts',(-0.712553859124697,0.888397715677925,
11.5699732202525));
#8358=CARTESIAN_POINT('Ctrl Pts',(-1.1131339679836,0.251233314201274,11.6280728566751));
#8359=CARTESIAN_POINT('Ctrl Pts',(-1.02901641656587,-0.498400062976102,
11.6862845413367));
#8360=CARTESIAN_POINT('Ctrl Pts',(-0.494901381262588,-1.03273028842869,
11.7445959726463));
#8361=CARTESIAN_POINT('Ctrl Pts',(0.256963427041344,-1.11790522486644,11.8030028921807));
#8362=CARTESIAN_POINT('Ctrl Pts',(0.898645546609871,-0.714501447365378,
11.8614828340231));
#8363=CARTESIAN_POINT('Ctrl Pts',(1.06558957851034,-0.237981063051787,11.900531417317));
#8364=CARTESIAN_POINT('Ctrl Pts',(1.0656219039434,0.00161635137504347,11.9200480207597));
#8365=CARTESIAN_POINT('Ctrl Pts',(0.970174595120126,-0.00503563731106881,
8.92177107464792));
#8366=CARTESIAN_POINT('Ctrl Pts',(0.97014513332141,0.213336147360704,8.93955872692312));
#8367=CARTESIAN_POINT('Ctrl Pts',(0.818084749800134,0.646712210522538,8.97507667223915));
#8368=CARTESIAN_POINT('Ctrl Pts',(0.235394562966291,1.01281040837635,9.02817474980784));
#8369=CARTESIAN_POINT('Ctrl Pts',(-0.445899628158482,0.93542064652562,9.08109684256912));
#8370=CARTESIAN_POINT('Ctrl Pts',(-0.92891112461198,0.451907699888587,9.13385094731592));
#8371=CARTESIAN_POINT('Ctrl Pts',(-1.00493384222522,-0.225268939789807,
9.18644257275678));
#8372=CARTESIAN_POINT('Ctrl Pts',(-0.642976055403776,-0.800405537674571,
9.23888044258555));
#8373=CARTESIAN_POINT('Ctrl Pts',(-0.190252948988789,-0.958506313741143,
9.27591831988632));
#8374=CARTESIAN_POINT('Ctrl Pts',(0.0760513139059781,-0.947021503110477,
9.29767447763811));
#8375=CARTESIAN_POINT('Ctrl Pts',(0.181774589175,-0.933637477829087,9.30637415940269));
#8376=CARTESIAN_POINT('Ctrl Pts',(0.311077731563098,-0.900290110612741,
9.31724319560765));
#8377=CARTESIAN_POINT('Ctrl Pts',(0.457151798821983,-0.834835030372344,
9.33027774261818));
#8378=CARTESIAN_POINT('Ctrl Pts',(0.703776523677854,-0.670467504751259,
9.35440044234417));
#8379=CARTESIAN_POINT('Ctrl Pts',(0.957142808831923,-0.298758897479058,
9.38956627149585));
#8380=CARTESIAN_POINT('Ctrl Pts',(0.957424510406942,0.292287109831173,9.43571919831589));
#8381=CARTESIAN_POINT('Ctrl Pts',(0.652789107737886,0.738706737228365,9.47794167639263));
#8382=CARTESIAN_POINT('Ctrl Pts',(0.218804460523358,0.946882426971243,9.51626539400664));
#8383=CARTESIAN_POINT('Ctrl Pts',(-0.213532779418316,0.947038202528517,
9.55071209496058));
#8384=CARTESIAN_POINT('Ctrl Pts',(-0.602655482246472,0.759384664282859,
9.58511969001727));
#8385=CARTESIAN_POINT('Ctrl Pts',(-0.871589920010413,0.42210069020356,9.61948765332899));
#8386=CARTESIAN_POINT('Ctrl Pts',(-0.967523567997481,0.00184733610570532,
9.653821175649));
#8387=CARTESIAN_POINT('Ctrl Pts',(-0.887562212018797,-0.347914027050768,
9.68240518610407));
#8388=CARTESIAN_POINT('Ctrl Pts',(-0.737597515612331,-0.586165380726041,
9.70525951581694));
#8389=CARTESIAN_POINT('Ctrl Pts',(-0.538767917261371,-0.785303060437251,
9.72810483743237));
#8390=CARTESIAN_POINT('Ctrl Pts',(-0.216019756644109,-0.940798544572053,
9.75664373683193));
#8391=CARTESIAN_POINT('Ctrl Pts',(0.213607429628279,-0.940753217150432,
9.7908691867679));
#8392=CARTESIAN_POINT('Ctrl Pts',(0.60059962902176,-0.754427589325977,9.8250751579334));
#8393=CARTESIAN_POINT('Ctrl Pts',(0.867933207756893,-0.418899848761693,
9.85926601803759));
#8394=CARTESIAN_POINT('Ctrl Pts',(0.974739488850976,0.0459663586074821,
9.89724109276077));
#8395=CARTESIAN_POINT('Ctrl Pts',(0.816946688402954,0.556586882372049,9.93900235474234));
#8396=CARTESIAN_POINT('Ctrl Pts',(0.43728553409625,0.859707800736691,9.97695998576935));
#8397=CARTESIAN_POINT('Ctrl Pts',(0.0705800023320674,0.9425400029561,10.0073260394253));
#8398=CARTESIAN_POINT('Ctrl Pts',(-0.304294465461892,0.915163773381358,
10.0376942387437));
#8399=CARTESIAN_POINT('Ctrl Pts',(-0.725224446706966,0.672378460587817,
10.0756555841161));
#8400=CARTESIAN_POINT('Ctrl Pts',(-0.978574572485742,0.146870510254935,
10.1212292346273));
#8401=CARTESIAN_POINT('Ctrl Pts',(-0.888584387525938,-0.454575686059261,
10.1687245791249));
#8402=CARTESIAN_POINT('Ctrl Pts',(-0.435769223197817,-0.907990577502227,
10.2181541230081));
#8403=CARTESIAN_POINT('Ctrl Pts',(0.152021146808637,-0.973556519824532,
10.263825841961));
#8404=CARTESIAN_POINT('Ctrl Pts',(0.604566615086981,-0.754940950053836,
10.3038313663868));
#8405=CARTESIAN_POINT('Ctrl Pts',(0.872819826465687,-0.418341246999725,
10.3381524858387));
#8406=CARTESIAN_POINT('Ctrl Pts',(0.985741421500406,0.0724135376997006,
10.3782322375385));
#8407=CARTESIAN_POINT('Ctrl Pts',(0.790438866129083,0.633079182429389,10.4240968327084));
#8408=CARTESIAN_POINT('Ctrl Pts',(0.223085878751149,0.989766778797461,10.475788493229));
#8409=CARTESIAN_POINT('Ctrl Pts',(-0.443636411700346,0.91478193674211,10.527582683884));
#8410=CARTESIAN_POINT('Ctrl Pts',(-0.919485443943618,0.43944156877107,10.5794894871194));
#8411=CARTESIAN_POINT('Ctrl Pts',(-0.995164253076116,-0.230475400336733,
10.6315180175327));
#8412=CARTESIAN_POINT('Ctrl Pts',(-0.635988207832033,-0.802768774991268,
10.6836769758179));
#8413=CARTESIAN_POINT('Ctrl Pts',(0.00372743422999969,-1.02704830689769,
10.7359754361821));
#8414=CARTESIAN_POINT('Ctrl Pts',(0.537816073043853,-0.839863792888686,
10.7796792126973));
#8415=CARTESIAN_POINT('Ctrl Pts',(0.826941185002114,-0.51471177031735,10.8147214066431));
#8416=CARTESIAN_POINT('Ctrl Pts',(0.994767696821434,-0.11252633051923,10.8498165152454));
#8417=CARTESIAN_POINT('Ctrl Pts',(0.932614102397896,0.453135513169429,10.893785840357));
#8418=CARTESIAN_POINT('Ctrl Pts',(0.446931472105046,0.938895669176947,10.9467167749459));
#8419=CARTESIAN_POINT('Ctrl Pts',(-0.160185357817544,1.00689283818422,10.9939220689488));
#8420=CARTESIAN_POINT('Ctrl Pts',(-0.62876276007964,0.780495118745785,11.0353450150309));
#8421=CARTESIAN_POINT('Ctrl Pts',(-0.907457292336147,0.431620682347231,
11.0709316429417));
#8422=CARTESIAN_POINT('Ctrl Pts',(-1.00706550093635,-0.00502807237038878,
11.1066026010044));
#8423=CARTESIAN_POINT('Ctrl Pts',(-0.907333018059293,-0.442590496284849,
11.1423573938483));
#8424=CARTESIAN_POINT('Ctrl Pts',(-0.626930395137068,-0.794427236840942,
11.1781982571942));
#8425=CARTESIAN_POINT('Ctrl Pts',(-0.220647298824694,-0.990289626669596,
11.2141257343577));
#8426=CARTESIAN_POINT('Ctrl Pts',(0.231426710381895,-0.990273776039337,
11.2501419138969));
#8427=CARTESIAN_POINT('Ctrl Pts',(0.639831749928173,-0.793739088548,11.2862464373884));
#8428=CARTESIAN_POINT('Ctrl Pts',(0.923168828792549,-0.43866823784993,11.3224405845602));
#8429=CARTESIAN_POINT('Ctrl Pts',(1.0247318209223,0.0054897969252295,11.3587249749106));
#8430=CARTESIAN_POINT('Ctrl Pts',(0.923067333024604,0.450369874564741,11.3951000868224));
#8431=CARTESIAN_POINT('Ctrl Pts',(0.590716128822805,0.868819753923387,11.4376441375946));
#8432=CARTESIAN_POINT('Ctrl Pts',(-0.00492338137778625,1.0783947024351,
11.4864178746861));
#8433=CARTESIAN_POINT('Ctrl Pts',(-0.678977034279962,0.842905562412496,
11.5414947246563));
#8434=CARTESIAN_POINT('Ctrl Pts',(-1.06028826449987,0.236776613170064,11.5967771211505));
#8435=CARTESIAN_POINT('Ctrl Pts',(-0.980329318877891,-0.477775118277444,
11.6522652599988));
#8436=CARTESIAN_POINT('Ctrl Pts',(-0.470413594001006,-0.988225256329599,
11.7079556521475));
#8437=CARTESIAN_POINT('Ctrl Pts',(0.249062373267229,-1.06999291276201,11.7638509027688));
#8438=CARTESIAN_POINT('Ctrl Pts',(0.864611352792192,-0.683332131784587,
11.8199382283231));
#8439=CARTESIAN_POINT('Ctrl Pts',(1.02527007578566,-0.225384236483218,11.8574728609456));
#8440=CARTESIAN_POINT('Ctrl Pts',(1.02530118372115,0.00518903684214906,
11.8762543955908));
#8441=CARTESIAN_POINT('Ctrl Pts',(1.02975721923246,-0.00501326104248905,
8.92159505735362));
#8442=CARTESIAN_POINT('Ctrl Pts',(1.02972597594797,0.226562952611486,8.94045828718835));
#8443=CARTESIAN_POINT('Ctrl Pts',(0.86837094344991,0.686546493545894,8.97815772733461));
#8444=CARTESIAN_POINT('Ctrl Pts',(0.25006196000382,1.0749630458525,9.03449802178365));
#8445=CARTESIAN_POINT('Ctrl Pts',(-0.472771913624819,0.992854014976237,
9.09065090430009));
#8446=CARTESIAN_POINT('Ctrl Pts',(-0.985019752728312,0.479982040438132,
9.14660306370138));
#8447=CARTESIAN_POINT('Ctrl Pts',(-1.06552888416002,-0.237875691236344,
9.2023562706398));
#8448=CARTESIAN_POINT('Ctrl Pts',(-0.682010172306705,-0.847083596841777,
9.25790631176331));
#8449=CARTESIAN_POINT('Ctrl Pts',(-0.202814134616569,-1.01433803010485,
9.29710989140601));
#8450=CARTESIAN_POINT('Ctrl Pts',(0.0788679011663583,-1.00218874924703,
9.32012268492401));
#8451=CARTESIAN_POINT('Ctrl Pts',(0.190681245832686,-0.988033404006502,
9.32932353240439));
#8452=CARTESIAN_POINT('Ctrl Pts',(0.327404814279713,-0.952769801991741,
9.34081658256902));
#8453=CARTESIAN_POINT('Ctrl Pts',(0.481815903298182,-0.883576107595531,
9.35459540007272));
#8454=CARTESIAN_POINT('Ctrl Pts',(0.742439859809724,-0.709871646472506,
9.38008794825078));
#8455=CARTESIAN_POINT('Ctrl Pts',(1.00993756139607,-0.317273228204009,9.417228448983));
#8456=CARTESIAN_POINT('Ctrl Pts',(1.0101057984205,0.30611713919737,9.46590779494714));
#8457=CARTESIAN_POINT('Ctrl Pts',(0.68913686078465,0.776249633888103,9.51038260407111));
#8458=CARTESIAN_POINT('Ctrl Pts',(0.232608623129516,0.995159965668924,9.55069684565993));
#8459=CARTESIAN_POINT('Ctrl Pts',(-0.221612783036091,0.995256986950812,
9.58688996014151));
#8460=CARTESIAN_POINT('Ctrl Pts',(-0.629867340389913,0.798302867057984,
9.62299299529222));
#8461=CARTESIAN_POINT('Ctrl Pts',(-0.911611061773582,0.444834495495162,
9.65900815200399));
#8462=CARTESIAN_POINT('Ctrl Pts',(-1.01191808941633,0.00508561341048963,
9.69493535750616));
#8463=CARTESIAN_POINT('Ctrl Pts',(-0.928311649430149,-0.360330144567805,
9.72480279674522));
#8464=CARTESIAN_POINT('Ctrl Pts',(-0.771806399654962,-0.608946941831366,
9.74865322870009));
#8465=CARTESIAN_POINT('Ctrl Pts',(-0.56447207066945,-0.81658281100874,9.77247530670478));
#8466=CARTESIAN_POINT('Ctrl Pts',(-0.228304054980772,-0.97846315009502,
9.80220116775789));
#8467=CARTESIAN_POINT('Ctrl Pts',(0.218386224671673,-0.97832648895643,9.83778856842642));
#8468=CARTESIAN_POINT('Ctrl Pts',(0.62000742826206,-0.784853582088767,9.87329465940624));
#8469=CARTESIAN_POINT('Ctrl Pts',(0.896904593067191,-0.437180626270341,
9.90872029217887));
#8470=CARTESIAN_POINT('Ctrl Pts',(1.00724607137228,0.0435831230782877,9.94799570611922));
#8471=CARTESIAN_POINT('Ctrl Pts',(0.844239597184889,0.57038071251276,9.99108817060923));
#8472=CARTESIAN_POINT('Ctrl Pts',(0.453398116619752,0.882165967328861,10.0301536130233));
#8473=CARTESIAN_POINT('Ctrl Pts',(0.0767926029015151,0.96719411053426,10.0613423168352));
#8474=CARTESIAN_POINT('Ctrl Pts',(-0.307678099377883,0.939075809396451,
10.0924888336935));
#8475=CARTESIAN_POINT('Ctrl Pts',(-0.738398945185493,0.690405637103079,
10.1313486661221));
#8476=CARTESIAN_POINT('Ctrl Pts',(-0.996717094215216,0.153989961224338,
10.1778602455462));
#8477=CARTESIAN_POINT('Ctrl Pts',(-0.904871139950366,-0.457998784943317,
10.2261955249004));
#8478=CARTESIAN_POINT('Ctrl Pts',(-0.445258050472082,-0.917694255083475,
10.2763447701295));
#8479=CARTESIAN_POINT('Ctrl Pts',(0.149034788405817,-0.983646387217854,
10.3225265250447));
#8480=CARTESIAN_POINT('Ctrl Pts',(0.605170989433338,-0.76314561160354,10.3628581184876));
#8481=CARTESIAN_POINT('Ctrl Pts',(0.874893609330296,-0.424537808037555,
10.3973795175289));
#8482=CARTESIAN_POINT('Ctrl Pts',(0.988072988143918,0.0679732521261451,
10.4376022678486));
#8483=CARTESIAN_POINT('Ctrl Pts',(0.792326107474424,0.628891245980529,10.4835024209011));
#8484=CARTESIAN_POINT('Ctrl Pts',(0.226370211101435,0.984231506720089,10.5350532100885));
#8485=CARTESIAN_POINT('Ctrl Pts',(-0.436123968807799,0.909336880303367,
10.5865289946361));
#8486=CARTESIAN_POINT('Ctrl Pts',(-0.907099616963547,0.438321024396503,
10.6379399044686));
#8487=CARTESIAN_POINT('Ctrl Pts',(-0.981413923118005,-0.222912321612607,
10.6892968715003));
#8488=CARTESIAN_POINT('Ctrl Pts',(-0.627778574641029,-0.785671011073721,
10.7406112122533));
#8489=CARTESIAN_POINT('Ctrl Pts',(-0.000441041026566889,-1.00521891170418,
10.7918931531218));
#8490=CARTESIAN_POINT('Ctrl Pts',(0.52144028745575,-0.822006313423052,10.8346123836516));
#8491=CARTESIAN_POINT('Ctrl Pts',(0.803284290233143,-0.504957992571902,
10.8687804323078));
#8492=CARTESIAN_POINT('Ctrl Pts',(0.966617256853383,-0.113399258972559,
10.9029470303529));
#8493=CARTESIAN_POINT('Ctrl Pts',(0.905970307108542,0.43601079523538,10.9456579859439));
#8494=CARTESIAN_POINT('Ctrl Pts',(0.435368363134417,0.906210162272629,10.9969260175495));
#8495=CARTESIAN_POINT('Ctrl Pts',(-0.150964337688312,0.971610417839796,
11.0425194902371));
#8496=CARTESIAN_POINT('Ctrl Pts',(-0.602400284855791,0.753381994777755,
11.0824343495858));
#8497=CARTESIAN_POINT('Ctrl Pts',(-0.870405218502895,0.417758929984093,
11.1166674917653));
#8498=CARTESIAN_POINT('Ctrl Pts',(-0.965973798101014,-0.00153480929624971,
11.1509206149028));
#8499=CARTESIAN_POINT('Ctrl Pts',(-0.870284764404151,-0.421002164664357,
11.1852011748759));
#8500=CARTESIAN_POINT('Ctrl Pts',(-0.601830888141152,-0.757731064011876,
11.2195098193561));
#8501=CARTESIAN_POINT('Ctrl Pts',(-0.213486681158965,-0.944867152397458,
11.2538513120739));
#8502=CARTESIAN_POINT('Ctrl Pts',(0.217961288027539,-0.9447880279063,11.2882255611698));
#8503=CARTESIAN_POINT('Ctrl Pts',(0.607187071933093,-0.757413281709361,
11.3226393123278));
#8504=CARTESIAN_POINT('Ctrl Pts',(0.876844610743522,-0.419393441672649,
11.3570938790573));
#8505=CARTESIAN_POINT('Ctrl Pts',(0.973349361765023,0.00288962313001501,
11.3915922816714));
#8506=CARTESIAN_POINT('Ctrl Pts',(0.876757888575241,0.425354250291934,11.4261375530626));
#8507=CARTESIAN_POINT('Ctrl Pts',(0.561431004887934,0.822273741287479,11.4664977820191));
#8508=CARTESIAN_POINT('Ctrl Pts',(-0.0029686874240922,1.02071711991479,
11.5127131391255));
#8509=CARTESIAN_POINT('Ctrl Pts',(-0.64073387394736,0.797757518731472,11.5648313598225));
#8510=CARTESIAN_POINT('Ctrl Pts',(-1.00104023104205,0.224805257101963,11.6170855603212));
#8511=CARTESIAN_POINT('Ctrl Pts',(-0.925442327878976,-0.449927244069821,
11.6694834791769));
#8512=CARTESIAN_POINT('Ctrl Pts',(-0.444252973113854,-0.931505251605332,
11.7220333653095));
#8513=CARTESIAN_POINT('Ctrl Pts',(0.234224731061071,-1.00859451570503,11.7747423231968));
#8514=CARTESIAN_POINT('Ctrl Pts',(0.81445437030024,-0.644038197480611,11.827617902194));
#8515=CARTESIAN_POINT('Ctrl Pts',(0.965855550860405,-0.212574361888019,
11.8629834282669));
#8516=CARTESIAN_POINT('Ctrl Pts',(0.96588488284949,0.00483552499042606,
11.8806927284981));
#8517=CARTESIAN_POINT('Ctrl Pts',(1.06707985315926,-0.00123476537768325,
8.87526981796726));
#8518=CARTESIAN_POINT('Ctrl Pts',(1.06704748827009,0.238654817693568,8.89481022010543));
#8519=CARTESIAN_POINT('Ctrl Pts',(0.8998395871503,0.715860547817637,8.93391958700505));
#8520=CARTESIAN_POINT('Ctrl Pts',(0.257138893203379,1.11993605733771,8.99249828235584));
#8521=CARTESIAN_POINT('Ctrl Pts',(-0.496179770892746,1.03467055578583,9.05102018674564));
#8522=CARTESIAN_POINT('Ctrl Pts',(-1.03136334290367,0.499226173485843,9.10945853061635));
#8523=CARTESIAN_POINT('Ctrl Pts',(-1.11588620841635,-0.25201787262317,9.16781107428167));
#8524=CARTESIAN_POINT('Ctrl Pts',(-0.713942264474925,-0.890966581948507,
9.22606298427746));
#8525=CARTESIAN_POINT('Ctrl Pts',(-0.21059029264254,-1.06682548550579,9.26725052311974));
#8526=CARTESIAN_POINT('Ctrl Pts',(0.0855976314555819,-1.054052987163,9.29144852924291));
#8527=CARTESIAN_POINT('Ctrl Pts',(0.203192078226194,-1.03916618931912,9.30112514367417));
#8528=CARTESIAN_POINT('Ctrl Pts',(0.347031573799707,-1.00207044132561,9.31321650524867));
#8529=CARTESIAN_POINT('Ctrl Pts',(0.509545413954052,-0.929248527148037,
9.32771837457598));
#8530=CARTESIAN_POINT('Ctrl Pts',(0.783953494823923,-0.746364639224551,
9.35455933228035));
#8531=CARTESIAN_POINT('Ctrl Pts',(1.06593687748999,-0.332681687964893,9.39370140995972));
#8532=CARTESIAN_POINT('Ctrl Pts',(1.06623597197503,0.325089931912099,9.44506593995741));
#8533=CARTESIAN_POINT('Ctrl Pts',(0.727258506600483,0.821784451489806,9.49204879073065));
#8534=CARTESIAN_POINT('Ctrl Pts',(0.244580458213156,1.05328946139207,9.53467422595177));
#8535=CARTESIAN_POINT('Ctrl Pts',(-0.236010419637293,1.05343265745285,9.57296888983229));
#8536=CARTESIAN_POINT('Ctrl Pts',(-0.668252297750573,0.84494474001119,9.61119194755577));
#8537=CARTESIAN_POINT('Ctrl Pts',(-0.96672974583056,0.47053384886532,9.64934284697546));
#8538=CARTESIAN_POINT('Ctrl Pts',(-1.07306322407242,0.00448821120086209,
9.68741884390622));
#8539=CARTESIAN_POINT('Ctrl Pts',(-0.98443925125814,-0.382945442280808,
9.71908515419177));
#8540=CARTESIAN_POINT('Ctrl Pts',(-0.818466620582291,-0.646608252509767,
9.74437859502403));
#8541=CARTESIAN_POINT('Ctrl Pts',(-0.598557383662294,-0.866842730767591,
9.76964562480785));
#8542=CARTESIAN_POINT('Ctrl Pts',(-0.241936616572021,-1.03858706068224,
9.8011796330524));
#8543=CARTESIAN_POINT('Ctrl Pts',(0.232022932609555,-1.03845317207481,9.83893862551647));
#8544=CARTESIAN_POINT('Ctrl Pts',(0.658205813052732,-0.833156021220092,
9.87661449080378));
#8545=CARTESIAN_POINT('Ctrl Pts',(0.952040531211175,-0.464218655543736,
9.91420589839601));
#8546=CARTESIAN_POINT('Ctrl Pts',(1.06912457221153,0.0459190084133642,9.95587871432431));
#8547=CARTESIAN_POINT('Ctrl Pts',(0.896163985835651,0.604804501827073,10.0015953006467));
#8548=CARTESIAN_POINT('Ctrl Pts',(0.481633120790058,0.935455264202716,10.0430249679984));
#8549=CARTESIAN_POINT('Ctrl Pts',(0.0823590282165599,1.02559253520912,10.0760894895048));
#8550=CARTESIAN_POINT('Ctrl Pts',(-0.325147597322649,0.995783918629276,
10.1091010377242));
#8551=CARTESIAN_POINT('Ctrl Pts',(-0.781419164358984,0.732302037853845,
10.1502641539734));
#8552=CARTESIAN_POINT('Ctrl Pts',(-1.05481197310381,0.164416196982754,10.1994999089072));
#8553=CARTESIAN_POINT('Ctrl Pts',(-0.957579147098405,-0.482838702730343,
10.2506175062341));
#8554=CARTESIAN_POINT('Ctrl Pts',(-0.471923124685282,-0.968373088850138,
10.3035915305234));
#8555=CARTESIAN_POINT('Ctrl Pts',(0.155063724599384,-1.03780443842841,10.3523070394179));
#8556=CARTESIAN_POINT('Ctrl Pts',(0.635656486568682,-0.80540414765001,10.3948019151775));
#8557=CARTESIAN_POINT('Ctrl Pts',(0.919506135055416,-0.448974992668351,
10.431135292655));
#8558=CARTESIAN_POINT('Ctrl Pts',(1.03842188491753,0.0688216676404025,10.4734179726515));
#8559=CARTESIAN_POINT('Ctrl Pts',(0.832773812963301,0.657512741565147,10.5215893003721));
#8560=CARTESIAN_POINT('Ctrl Pts',(0.239794832763951,1.02952139718656,10.5755830086345));
#8561=CARTESIAN_POINT('Ctrl Pts',(-0.45262480578768,0.950973831099203,10.6293794921735));
#8562=CARTESIAN_POINT('Ctrl Pts',(-0.943549992884528,0.459607520916314,
10.6829827001157));
#8563=CARTESIAN_POINT('Ctrl Pts',(-1.0205554561502,-0.228234505928641,10.7363967638958));
#8564=CARTESIAN_POINT('Ctrl Pts',(-0.653411141648812,-0.8119181268805,10.7896259939305));
#8565=CARTESIAN_POINT('Ctrl Pts',(-0.00424388176717446,-1.0387549035362,
10.842676676515));
#8566=CARTESIAN_POINT('Ctrl Pts',(0.534047985812385,-0.849488279944819,
10.8867394772746));
#8567=CARTESIAN_POINT('Ctrl Pts',(0.824125963852387,-0.523093463830685,
10.9219091864479));
#8568=CARTESIAN_POINT('Ctrl Pts',(0.991956861439558,-0.120598140671722,
10.9570246594903));
#8569=CARTESIAN_POINT('Ctrl Pts',(0.929487999659989,0.442783713789643,11.0008170365044));
#8570=CARTESIAN_POINT('Ctrl Pts',(0.448174079732207,0.923135490503192,11.0532130656101));
#8571=CARTESIAN_POINT('Ctrl Pts',(-0.149246274677376,0.989455764861352,
11.099658036704));
#8572=CARTESIAN_POINT('Ctrl Pts',(-0.607887737979885,0.767591199020883,
11.1402120021755));
#8573=CARTESIAN_POINT('Ctrl Pts',(-0.879518432239106,0.427263871776012,
11.174912490265));
#8574=CARTESIAN_POINT('Ctrl Pts',(-0.976082172216738,0.00308668187306984,
11.2095606056502));
#8575=CARTESIAN_POINT('Ctrl Pts',(-0.879406973557938,-0.420236621178114,
11.2441531370345));
#8576=CARTESIAN_POINT('Ctrl Pts',(-0.608997527935039,-0.759237523513902,
11.2786964846213));
#8577=CARTESIAN_POINT('Ctrl Pts',(-0.218810131166539,-0.947139071472111,
11.3131910809694));
#8578=CARTESIAN_POINT('Ctrl Pts',(0.213658136544478,-0.94694361480508,11.3476445942225));
#8579=CARTESIAN_POINT('Ctrl Pts',(0.602841583902335,-0.759465040168191,
11.3820544328846));
#8580=CARTESIAN_POINT('Ctrl Pts',(0.871796157798383,-0.422143654068603,
11.4164262050128));
#8581=CARTESIAN_POINT('Ctrl Pts',(0.967743919091153,-0.0017645367439769,
11.4507628656491));
#8582=CARTESIAN_POINT('Ctrl Pts',(0.87170737632655,0.417779623846008,11.4850673080446));
#8583=CARTESIAN_POINT('Ctrl Pts',(0.559133149320638,0.811009041168935,11.5250561770006));
#8584=CARTESIAN_POINT('Ctrl Pts',(0.00135353631370101,1.00676598110684,
11.5707114011782));
#8585=CARTESIAN_POINT('Ctrl Pts',(-0.626564919774301,0.786837182071727,
11.6220280050714));
#8586=CARTESIAN_POINT('Ctrl Pts',(-0.97989246930752,0.224284866953415,11.6733084179627));
#8587=CARTESIAN_POINT('Ctrl Pts',(-0.905576830269774,-0.435795198091819,
11.7245632840688));
#8588=CARTESIAN_POINT('Ctrl Pts',(-0.436058105615478,-0.905191005915266,
11.7758062366315));
#8589=CARTESIAN_POINT('Ctrl Pts',(0.223607192099306,-0.979837529970289,
11.8270420788981));
#8590=CARTESIAN_POINT('Ctrl Pts',(0.785864651600639,-0.626123961781889,
11.8782964306891));
#8591=CARTESIAN_POINT('Ctrl Pts',(0.931965422655655,-0.209149242308135,
11.9124623274458));
#8592=CARTESIAN_POINT('Ctrl Pts',(0.931993756029,0.000858864397959647,11.9295687096166));
#8593=CARTESIAN_POINT('Ctrl Pts',(1.05361350283538,0.00348296873761165,
8.81732980737331));
#8594=CARTESIAN_POINT('Ctrl Pts',(1.0535815233416,0.24051598896115,8.836637525849));
#8595=CARTESIAN_POINT('Ctrl Pts',(0.888483313940475,0.712467681174716,8.8753039923388));
#8596=CARTESIAN_POINT('Ctrl Pts',(0.251129926275458,1.11367978850147,8.93341429944556));
#8597=CARTESIAN_POINT('Ctrl Pts',(-0.498485108509924,1.0291918195949,8.99163796243809));
#8598=CARTESIAN_POINT('Ctrl Pts',(-1.03291163235678,0.495047846251041,9.04996025164164));
#8599=CARTESIAN_POINT('Ctrl Pts',(-1.11791454965682,-0.257013855216408,
9.10837309877508));
#8600=CARTESIAN_POINT('Ctrl Pts',(-0.714602934220277,-0.898858458114211,
9.16686610473355));
#8601=CARTESIAN_POINT('Ctrl Pts',(-0.207691595850096,-1.07623821818795,
9.20834669901183));
#8602=CARTESIAN_POINT('Ctrl Pts',(0.0911678852700241,-1.06335197381873,
9.23276211443464));
#8603=CARTESIAN_POINT('Ctrl Pts',(0.209866246985131,-1.04832623169789,9.24252954635982));
#8604=CARTESIAN_POINT('Ctrl Pts',(0.355138049245429,-1.01086646870226,9.25474086067091));
#8605=CARTESIAN_POINT('Ctrl Pts',(0.519396104990609,-0.937268700996166,
9.26939783627726));
#8606=CARTESIAN_POINT('Ctrl Pts',(0.796954605660454,-0.752300466043746,
9.29654620334218));
#8607=CARTESIAN_POINT('Ctrl Pts',(1.08280563220712,-0.333290926636967,9.3361995653769));
#8608=CARTESIAN_POINT('Ctrl Pts',(1.08337830847036,0.334912126982432,9.38837847049749));
#8609=CARTESIAN_POINT('Ctrl Pts',(0.738315461087922,0.840931330660767,9.43622874255615));
#8610=CARTESIAN_POINT('Ctrl Pts',(0.245636643115447,1.07736261426428,9.47973966869423));
#8611=CARTESIAN_POINT('Ctrl Pts',(-0.245887374235519,1.07760739558264,9.51890418887534));
#8612=CARTESIAN_POINT('Ctrl Pts',(-0.688848319885635,0.864061693882516,
9.55807043542996));
#8613=CARTESIAN_POINT('Ctrl Pts',(-0.995336775626925,0.479757650920096,
9.59723465260094));
#8614=CARTESIAN_POINT('Ctrl Pts',(-1.10479102070153,0.000469460247281091,
9.63639363908221));
#8615=CARTESIAN_POINT('Ctrl Pts',(-1.01355573715264,-0.398724027650001,
9.66901900999136));
#8616=CARTESIAN_POINT('Ctrl Pts',(-0.842337462850113,-0.670747199386004,
9.69511336499282));
#8617=CARTESIAN_POINT('Ctrl Pts',(-0.615278718012576,-0.898162572142696,
9.72120320245627));
#8618=CARTESIAN_POINT('Ctrl Pts',(-0.246601093264737,-1.07579559008464,
9.75380618018306));
#8619=CARTESIAN_POINT('Ctrl Pts',(0.244252856073734,-1.07574552507989,9.79291120095988));
#8620=CARTESIAN_POINT('Ctrl Pts',(0.686391851322618,-0.86285853975462,9.83199461216117));
#8621=CARTESIAN_POINT('Ctrl Pts',(0.991754530098738,-0.479576560375196,
9.87105294828468));
#8622=CARTESIAN_POINT('Ctrl Pts',(1.11368561614542,0.0512633874947476,9.91442019466662));
#8623=CARTESIAN_POINT('Ctrl Pts',(0.933546075553114,0.633941769683682,9.96207896521016));
#8624=CARTESIAN_POINT('Ctrl Pts',(0.500670512163495,0.979417458553777,10.0053529017601));
#8625=CARTESIAN_POINT('Ctrl Pts',(0.0830568987247602,1.07372340050911,10.0399368296195));
#8626=CARTESIAN_POINT('Ctrl Pts',(-0.34353856408149,1.04254504990199,10.0744958406771));
#8627=CARTESIAN_POINT('Ctrl Pts',(-0.821892667873493,0.766467885156324,
10.1176479867357));
#8628=CARTESIAN_POINT('Ctrl Pts',(-1.10907816859822,0.170284170765609,10.1693443469628));
#8629=CARTESIAN_POINT('Ctrl Pts',(-1.00698193012689,-0.510368802257205,
10.2231009495772));
#8630=CARTESIAN_POINT('Ctrl Pts',(-0.495623852462474,-1.02186283833792,
10.2788969581773));
#8631=CARTESIAN_POINT('Ctrl Pts',(0.165675816180989,-1.09524360987832,10.3302841789608));
#8632=CARTESIAN_POINT('Ctrl Pts',(0.673146867597226,-0.849907619411545,
10.3751549170633));
#8633=CARTESIAN_POINT('Ctrl Pts',(0.973126940522068,-0.473284873083087,
10.4135506217634));
#8634=CARTESIAN_POINT('Ctrl Pts',(1.0989251921748,0.0742805190588762,10.4582680283262));
#8635=CARTESIAN_POINT('Ctrl Pts',(0.881352975646305,0.697400663319528,10.5092599474022));
#8636=CARTESIAN_POINT('Ctrl Pts',(0.253250795230376,1.09155624924297,10.5664618213278));
#8637=CARTESIAN_POINT('Ctrl Pts',(-0.48074740256993,1.00836583230992,10.6234942829921));
#8638=CARTESIAN_POINT('Ctrl Pts',(-1.00144411702416,0.487271213800995,10.6803508700943));
#8639=CARTESIAN_POINT('Ctrl Pts',(-1.0831682514647,-0.242479183935224,10.7370260948775));
#8640=CARTESIAN_POINT('Ctrl Pts',(-0.693589794262895,-0.861829276622573,
10.7935153200748));
#8641=CARTESIAN_POINT('Ctrl Pts',(-0.00476094955930445,-1.10250820840403,
10.8498132155155));
#8642=CARTESIAN_POINT('Ctrl Pts',(0.566304342976761,-0.901685114817027,
10.8965673946933));
#8643=CARTESIAN_POINT('Ctrl Pts',(0.873933911656398,-0.55552423775986,10.9338691274573));
#8644=CARTESIAN_POINT('Ctrl Pts',(1.05187813310911,-0.128755879899797,10.9711041860801));
#8645=CARTESIAN_POINT('Ctrl Pts',(0.985595273517537,0.468350561132292,11.0175242489621));
#8646=CARTESIAN_POINT('Ctrl Pts',(0.475749928532382,0.977025441719225,11.0730273616305));
#8647=CARTESIAN_POINT('Ctrl Pts',(-0.156414893216963,1.04708636726262,11.1221822254832));
#8648=CARTESIAN_POINT('Ctrl Pts',(-0.641231356480644,0.812507364268063,
11.1650570351354));
#8649=CARTESIAN_POINT('Ctrl Pts',(-0.928115411763875,0.452991280889662,
11.2017171506232));
#8650=CARTESIAN_POINT('Ctrl Pts',(-1.02997376320952,0.00534914585065388,
11.2382833095929));
#8651=CARTESIAN_POINT('Ctrl Pts',(-0.927988165491989,-0.440956849896211,
11.2747605777941));
#8652=CARTESIAN_POINT('Ctrl Pts',(-0.643147665450665,-0.797961485702993,
11.3111461991335));
#8653=CARTESIAN_POINT('Ctrl Pts',(-0.232622271758171,-0.995586956799243,
11.3474425164299));
#8654=CARTESIAN_POINT('Ctrl Pts',(0.221782139701691,-0.995323011688169,
11.3836461234341));
#8655=CARTESIAN_POINT('Ctrl Pts',(0.630176503673988,-0.798514686074851,
11.4197621600222));
#8656=CARTESIAN_POINT('Ctrl Pts',(0.911993998160867,-0.444953718020728,
11.4557892580011));
#8657=CARTESIAN_POINT('Ctrl Pts',(1.0123375157838,-0.00499677880190555,
11.4917283504049));
#8658=CARTESIAN_POINT('Ctrl Pts',(0.911913781362388,0.433400322908333,11.5275805946167));
#8659=CARTESIAN_POINT('Ctrl Pts',(0.585711603391555,0.843623662983355,11.5693073793534));
#8660=CARTESIAN_POINT('Ctrl Pts',(0.00481853796942386,1.04723189572395,
11.6168567678419));
#8661=CARTESIAN_POINT('Ctrl Pts',(-0.647234763521536,0.818520165995884,
11.6701623256145));
#8662=CARTESIAN_POINT('Ctrl Pts',(-1.01294419891713,0.2356558517606,11.7232877007132));
#8663=CARTESIAN_POINT('Ctrl Pts',(-0.935844923634562,-0.446106838298428,
11.7762368087852));
#8664=CARTESIAN_POINT('Ctrl Pts',(-0.452045047065324,-0.929290107925388,
11.8290183926509));
#8665=CARTESIAN_POINT('Ctrl Pts',(0.225347069308191,-1.00558585215721,11.8816338257412));
#8666=CARTESIAN_POINT('Ctrl Pts',(0.800671735601205,-0.643237553051006,
11.9341015844704));
#8667=CARTESIAN_POINT('Ctrl Pts',(0.949567997660912,-0.217730099299315,
11.9689677728214));
#8668=CARTESIAN_POINT('Ctrl Pts',(0.949596863894161,-0.00377241348101253,
11.9863958711905));
#8669=CARTESIAN_POINT('Ctrl Pts',(1.01795130065334,0.00487363731203012,
8.80019806641107));
#8670=CARTESIAN_POINT('Ctrl Pts',(1.01792038659565,0.234009611419109,8.81886252453821));
#8671=CARTESIAN_POINT('Ctrl Pts',(0.858367966757573,0.690235048013234,8.85624002408532));
#8672=CARTESIAN_POINT('Ctrl Pts',(0.241569528156157,1.07870571562318,8.91248661418056));
#8673=CARTESIAN_POINT('Ctrl Pts',(-0.484837290617098,0.996972530018084,
8.96890545081248));
#8674=CARTESIAN_POINT('Ctrl Pts',(-1.00348249888983,0.478852252916471,9.02549359964913));
#8675=CARTESIAN_POINT('Ctrl Pts',(-1.08625117261773,-0.25179645236032,9.08224516844789));
#8676=CARTESIAN_POINT('Ctrl Pts',(-0.694018194752758,-0.876373474596457,
9.13915599966505));
#8677=CARTESIAN_POINT('Ctrl Pts',(-0.200132218465017,-1.04934671836633,
9.17957488341133));
#8678=CARTESIAN_POINT('Ctrl Pts',(0.0913368318045304,-1.03678149851834,
9.20338638692998));
#8679=CARTESIAN_POINT('Ctrl Pts',(0.207121875172981,-1.02212501822983,9.21291409202708));
#8680=CARTESIAN_POINT('Ctrl Pts',(0.348871161210955,-0.985577072042873,
9.22482919048418));
#8681=CARTESIAN_POINT('Ctrl Pts',(0.509211865524956,-0.913738037165839,
9.23913636256541));
#8682=CARTESIAN_POINT('Ctrl Pts',(0.780259255512014,-0.733117828399737,
9.26564749781129));
#8683=CARTESIAN_POINT('Ctrl Pts',(1.05975444985038,-0.323629573613465,9.30440431224551));
#8684=CARTESIAN_POINT('Ctrl Pts',(1.06047114568476,0.330478386785373,9.3554821017605));
#8685=CARTESIAN_POINT('Ctrl Pts',(0.722286003799723,0.826672635352907,9.40239348796624));
#8686=CARTESIAN_POINT('Ctrl Pts',(0.238614159531519,1.05887024839816,9.44510997373937));
#8687=CARTESIAN_POINT('Ctrl Pts',(-0.244534897444566,1.0591832153207,9.48360493669715));
#8688=CARTESIAN_POINT('Ctrl Pts',(-0.680524248557215,0.849074843118668,
9.52215116753634));
#8689=CARTESIAN_POINT('Ctrl Pts',(-0.98259760908771,0.470426970871326,9.56074113449322));
#8690=CARTESIAN_POINT('Ctrl Pts',(-1.09066217491685,-0.00244906966523479,
9.59937538820734));
#8691=CARTESIAN_POINT('Ctrl Pts',(-1.00058931413245,-0.396830955934259,
9.63160353230798));
#8692=CARTESIAN_POINT('Ctrl Pts',(-0.831280757584498,-0.66584407874337,
9.65740738981046));
#8693=CARTESIAN_POINT('Ctrl Pts',(-0.60660620885125,-0.890890186335246,
9.68322356907152));
#8694=CARTESIAN_POINT('Ctrl Pts',(-0.241464397156938,-1.06689249054125,
9.71551297140233));
#8695=CARTESIAN_POINT('Ctrl Pts',(0.245368155864266,-1.06692104952396,9.75429461177334));
#8696=CARTESIAN_POINT('Ctrl Pts',(0.684501955300456,-0.855569813249952,
9.79310524648812));
#8697=CARTESIAN_POINT('Ctrl Pts',(0.988229478846218,-0.474457482452504,
9.83194393027524));
#8698=CARTESIAN_POINT('Ctrl Pts',(1.10973816459222,0.0541175025352953,9.87512290940774));
#8699=CARTESIAN_POINT('Ctrl Pts',(0.930219960144453,0.635314767499316,9.92265302971509));
#8700=CARTESIAN_POINT('Ctrl Pts',(0.497804230880996,0.980626921647988,9.96588699941796));
#8701=CARTESIAN_POINT('Ctrl Pts',(0.0799630716897277,1.07501359287928,10.0004861839901));
#8702=CARTESIAN_POINT('Ctrl Pts',(-0.347252228161148,1.04382229510122,10.0350937644591));
#8703=CARTESIAN_POINT('Ctrl Pts',(-0.826997276535407,0.767113462252174,
10.0783561346641));
#8704=CARTESIAN_POINT('Ctrl Pts',(-1.11568341591399,0.168249508212943,10.1302891091875));
#8705=CARTESIAN_POINT('Ctrl Pts',(-1.01311996047222,-0.516807562056236,
10.1843847097011));
#8706=CARTESIAN_POINT('Ctrl Pts',(-0.497693146880373,-1.03272594487734,
10.2406345323798));
#8707=CARTESIAN_POINT('Ctrl Pts',(0.170406057393102,-1.10708621318768,10.2925411425343));
#8708=CARTESIAN_POINT('Ctrl Pts',(0.684033423898933,-0.858869402467361,
10.3379484762471));
#8709=CARTESIAN_POINT('Ctrl Pts',(0.988073809172079,-0.477253180864907,
10.3768544364604));
#8710=CARTESIAN_POINT('Ctrl Pts',(1.11580410768175,0.0783050484260798,10.4222217990858));
#8711=CARTESIAN_POINT('Ctrl Pts',(0.89490232388525,0.711594886645981,10.4740302655834));
#8712=CARTESIAN_POINT('Ctrl Pts',(0.255533065555895,1.11310545631092,10.5322604116042));
#8713=CARTESIAN_POINT('Ctrl Pts',(-0.493177190634868,1.028473309878,10.5904230992472));
#8714=CARTESIAN_POINT('Ctrl Pts',(-1.02539476057429,0.496166178496065,10.6485098680401));
#8715=CARTESIAN_POINT('Ctrl Pts',(-1.10926310066815,-0.250769149465673,
10.7065110803908));
#8716=CARTESIAN_POINT('Ctrl Pts',(-0.710019491092949,-0.885888782146993,
10.7644169839348));
#8717=CARTESIAN_POINT('Ctrl Pts',(-0.00271517191512337,-1.13323556057773,
10.8222205409864));
#8718=CARTESIAN_POINT('Ctrl Pts',(0.584651230956468,-0.926841543599498,
10.8702938955112));
#8719=CARTESIAN_POINT('Ctrl Pts',(0.901430071020036,-0.570430111687275,
10.9086978561871));
#8720=CARTESIAN_POINT('Ctrl Pts',(1.08480128691465,-0.130713242941942,10.9470608547078));
#8721=CARTESIAN_POINT('Ctrl Pts',(1.01658557007516,0.485161030998729,10.9949317431856));
#8722=CARTESIAN_POINT('Ctrl Pts',(0.490173403409379,1.01059242800624,11.0522381720562));
#8723=CARTESIAN_POINT('Ctrl Pts',(-0.163448336991982,1.08316288382942,11.103050538961));
#8724=CARTESIAN_POINT('Ctrl Pts',(-0.665244137705534,0.840414645124265,
11.1474196034443));
#8725=CARTESIAN_POINT('Ctrl Pts',(-0.962390571076912,0.468100768895086,
11.1853798655439));
#8726=CARTESIAN_POINT('Ctrl Pts',(-1.06798711473851,0.00416599671308398,
11.2232748034332));
#8727=CARTESIAN_POINT('Ctrl Pts',(-0.962266470067073,-0.458657680157008,
11.2610950285115));
#8728=CARTESIAN_POINT('Ctrl Pts',(-0.666738558731371,-0.829099316917844,
11.2988435852598));
#8729=CARTESIAN_POINT('Ctrl Pts',(-0.240581161310417,-1.03428058472939,
11.3365161841455));
#8730=CARTESIAN_POINT('Ctrl Pts',(0.23139593208825,-1.03402414691513,11.37411710958));
#8731=CARTESIAN_POINT('Ctrl Pts',(0.655753330921873,-0.829545509919698,
11.4116386576741));
#8732=CARTESIAN_POINT('Ctrl Pts',(0.948704829357944,-0.462037948503457,
11.4490826297383));
#8733=CARTESIAN_POINT('Ctrl Pts',(1.05305294362534,-0.00456577157253448,
11.4864478733918));
#8734=CARTESIAN_POINT('Ctrl Pts',(0.948608126586202,0.451416711858766,11.523733236039));
#8735=CARTESIAN_POINT('Ctrl Pts',(0.609246817799872,0.878201568608402,11.5671395812719));
#8736=CARTESIAN_POINT('Ctrl Pts',(0.00480141380439488,1.09007650729612,
11.6166080030503));
#8737=CARTESIAN_POINT('Ctrl Pts',(-0.673807025591558,0.852056511070549,
11.6720765353948));
#8738=CARTESIAN_POINT('Ctrl Pts',(-1.05440803560707,0.245435452705016,11.7273583516172));
#8739=CARTESIAN_POINT('Ctrl Pts',(-0.974155187242797,-0.464027523123006,
11.7824525288063));
#8740=CARTESIAN_POINT('Ctrl Pts',(-0.470784479502001,-0.966711922017756,
11.837360017147));
#8741=CARTESIAN_POINT('Ctrl Pts',(0.233728487300451,-1.0459922691019,11.8920770765874));
#8742=CARTESIAN_POINT('Ctrl Pts',(0.831757325146403,-0.66927695668899,11.9466131794695));
#8743=CARTESIAN_POINT('Ctrl Pts',(0.986370555206023,-0.227123217897721,
11.9828356523871));
#8744=CARTESIAN_POINT('Ctrl Pts',(0.986400528300369,-0.00496143295807807,
12.0009320223632));
#8745=CARTESIAN_POINT('Ctrl Pts',(0.999999342796208,0.0048712153097108,
8.80019806641107));
#8746=CARTESIAN_POINT('Ctrl Pts',(0.99996896462742,0.230035163961994,8.81853897995701));
#8747=CARTESIAN_POINT('Ctrl Pts',(0.843216945008081,0.678245689353448,8.85526000727444));
#8748=CARTESIAN_POINT('Ctrl Pts',(0.23714388778331,1.05999084182087,8.91053070559157));
#8749=CARTESIAN_POINT('Ctrl Pts',(-0.476746387578999,0.979670338171269,
8.96597705173729));
#8750=CARTESIAN_POINT('Ctrl Pts',(-0.98657616663209,0.470389879273211,9.0216024298575));
#8751=CARTESIAN_POINT('Ctrl Pts',(-1.06798165663575,-0.248000588468906,
9.07740270249169));
#8752=CARTESIAN_POINT('Ctrl Pts',(-0.682243081073035,-0.862304425765768,
9.1333764236107));
#8753=CARTESIAN_POINT('Ctrl Pts',(-0.196330490445415,-1.03251494397982,
9.17314484390509));
#8754=CARTESIAN_POINT('Ctrl Pts',(0.0904960552365201,-1.02015022040365,
9.19657718102618));
#8755=CARTESIAN_POINT('Ctrl Pts',(0.204441911777542,-1.00572651008441,9.20595357869542));
#8756=CARTESIAN_POINT('Ctrl Pts',(0.343951015893895,-0.96975630344906,9.21768054548145));
#8757=CARTESIAN_POINT('Ctrl Pts',(0.501773879908335,-0.899045416054097,
9.23176320323934));
#8758=CARTESIAN_POINT('Ctrl Pts',(0.768592409823833,-0.721243151610969,
9.2578611494339));
#8759=CARTESIAN_POINT('Ctrl Pts',(1.04382114359922,-0.318042243912805,9.29602676229045));
#8760=CARTESIAN_POINT('Ctrl Pts',(1.04456490155922,0.326294295864951,9.34634267499162));
#8761=CARTESIAN_POINT('Ctrl Pts',(0.711307557250243,0.815326125223123,9.39257751006242));
#8762=CARTESIAN_POINT('Ctrl Pts',(0.234442425347365,1.04427973165066,9.43469552996756));
#8763=CARTESIAN_POINT('Ctrl Pts',(-0.242097506080382,1.04460426316974,9.47266669612882));
#8764=CARTESIAN_POINT('Ctrl Pts',(-0.672296189994615,0.837312084419627,
9.51070107270169));
#8765=CARTESIAN_POINT('Ctrl Pts',(-0.970493141256397,0.463551157181226,
9.54879683116503));
#8766=CARTESIAN_POINT('Ctrl Pts',(-1.07723336834064,-0.00342794058422688,
9.58695206272228));
#8767=CARTESIAN_POINT('Ctrl Pts',(-0.988260429843343,-0.39307851175747,
9.61879599421848));
#8768=CARTESIAN_POINT('Ctrl Pts',(-0.82093539560644,-0.658946730224756,
9.64429884892662));
#8769=CARTESIAN_POINT('Ctrl Pts',(-0.598840710302034,-0.88141322392247,
9.66981982299092));
#8770=CARTESIAN_POINT('Ctrl Pts',(-0.237756057923814,-1.05547919442497,
9.70175433946707));
#8771=CARTESIAN_POINT('Ctrl Pts',(0.243905786180905,-1.05553040152794,9.74012683420727));
#8772=CARTESIAN_POINT('Ctrl Pts',(0.678604028637572,-0.846341399380819,
9.77854812145871));
#8773=CARTESIAN_POINT('Ctrl Pts',(0.979430107833126,-0.468912235308927,
9.81701586224876));
#8774=CARTESIAN_POINT('Ctrl Pts',(1.09985901046267,0.0548445677701001,9.85980673545165));
#8775=CARTESIAN_POINT('Ctrl Pts',(0.921933505746503,0.631124795915794,9.90693599171239));
#8776=CARTESIAN_POINT('Ctrl Pts',(0.4929126040201,0.973793160670524,9.94983738646297));
#8777=CARTESIAN_POINT('Ctrl Pts',(0.0780904371091028,1.06751269479759,9.98418939216924));
#8778=CARTESIAN_POINT('Ctrl Pts',(-0.346188348797786,1.0365452542535,10.0185609429505));
#8779=CARTESIAN_POINT('Ctrl Pts',(-0.822968443953264,0.76162232341949,10.0615600576428));
#8780=CARTESIAN_POINT('Ctrl Pts',(-1.11011929233597,0.166104281872854,10.1132080400722));
#8781=CARTESIAN_POINT('Ctrl Pts',(-1.0081246602054,-0.515708350877839,10.1670522944212));
#8782=CARTESIAN_POINT('Ctrl Pts',(-0.494775946618556,-1.02970801548153,
10.2230915794475));
#8783=CARTESIAN_POINT('Ctrl Pts',(0.171330015334639,-1.10394798748412,10.2748519542969));
#8784=CARTESIAN_POINT('Ctrl Pts',(0.683814393710209,-0.85633240678914,10.3201591760856));
#8785=CARTESIAN_POINT('Ctrl Pts',(0.987375224349673,-0.475369257557772,
10.3590026286433));
#8786=CARTESIAN_POINT('Ctrl Pts',(1.11501021817459,0.0796008030233853,10.4043267361272));
#8787=CARTESIAN_POINT('Ctrl Pts',(0.894257942603671,0.712772351603783,10.4561304980607));
#8788=CARTESIAN_POINT('Ctrl Pts',(0.254526418580225,1.11465334671006,10.5144063331842));
#8789=CARTESIAN_POINT('Ctrl Pts',(-0.495386650979013,1.03000796421648,10.5726689321936));
#8790=CARTESIAN_POINT('Ctrl Pts',(-1.02902006816757,0.496451864872819,10.6309084916996));
#8791=CARTESIAN_POINT('Ctrl Pts',(-1.11329107431628,-0.25302544687232,10.6891152782939));
#8792=CARTESIAN_POINT('Ctrl Pts',(-0.712411475504087,-0.890954531307481,
10.7472796615617));
#8793=CARTESIAN_POINT('Ctrl Pts',(-0.00144545535703713,-1.13970545531556,
10.8053921361455));
#8794=CARTESIAN_POINT('Ctrl Pts',(0.589562318042014,-0.932130645422847,
10.8537681412278));
#8795=CARTESIAN_POINT('Ctrl Pts',(0.908494555547074,-0.573322783618425,
10.8924337348326));
#8796=CARTESIAN_POINT('Ctrl Pts',(1.0932000203843,-0.130460109720627,10.9310743576345));
#8797=CARTESIAN_POINT('Ctrl Pts',(1.02452819258886,0.49024714203063,10.9793255246093));
#8798=CARTESIAN_POINT('Ctrl Pts',(0.493612168598575,1.02033558321459,11.037138824411));
#8799=CARTESIAN_POINT('Ctrl Pts',(-0.166230575259128,1.09368100121347,11.0884425957329));
#8800=CARTESIAN_POINT('Ctrl Pts',(-0.673140522140151,0.84850197959383,11.1332655331794));
#8801=CARTESIAN_POINT('Ctrl Pts',(-0.973483979429893,0.47222295927322,11.1716363210045));
#8802=CARTESIAN_POINT('Ctrl Pts',(-1.08028898641827,0.00311472479435195,
11.2099559586628));
#8803=CARTESIAN_POINT('Ctrl Pts',(-0.973354083483389,-0.465125791076451,
11.2482222395404));
#8804=CARTESIAN_POINT('Ctrl Pts',(-0.674252322492463,-0.840091585392608,
11.2864330284043));
#8805=CARTESIAN_POINT('Ctrl Pts',(-0.242715089956039,-1.04789098180051,
11.3245862592493));
#8806=CARTESIAN_POINT('Ctrl Pts',(0.23542767696283,-1.04765866302507,11.3626799542613));
#8807=CARTESIAN_POINT('Ctrl Pts',(0.665536159094464,-0.840435751119737,
11.4007121983223));
#8808=CARTESIAN_POINT('Ctrl Pts',(0.962591820228485,-0.467820172164233,
11.4386811727585));
#8809=CARTESIAN_POINT('Ctrl Pts',(1.06846208937938,-0.00379118886353965,
11.47658513569));
#8810=CARTESIAN_POINT('Ctrl Pts',(0.962501175338684,0.458913289962351,11.5144224357756));
#8811=CARTESIAN_POINT('Ctrl Pts',(0.618041205754224,0.892154566858533,11.5584863515166));
#8812=CARTESIAN_POINT('Ctrl Pts',(0.00421838652791971,1.10738146763147,
11.6087289304493));
#8813=CARTESIAN_POINT('Ctrl Pts',(-0.685284502455283,0.86560690604705,11.6650903417562));
#8814=CARTESIAN_POINT('Ctrl Pts',(-1.07219887432344,0.249028474249683,11.7212863124465));
#8815=CARTESIAN_POINT('Ctrl Pts',(-0.990640181337795,-0.472396051339649,
11.7773128627812));
#8816=CARTESIAN_POINT('Ctrl Pts',(-0.478640001005609,-0.983760746265736,
11.8331676524783));
#8817=CARTESIAN_POINT('Ctrl Pts',(0.238202676882345,-1.06445286799178,11.8888462567429));
#8818=CARTESIAN_POINT('Ctrl Pts',(0.846858663881909,-0.681098479204223,
11.9443505326692));
#8819=CARTESIAN_POINT('Ctrl Pts',(1.00427568511571,-0.230977292777482,11.9812290386622));
#8820=CARTESIAN_POINT('Ctrl Pts',(1.00430619197361,-0.004859230773597,11.9996476704237));
#8821=CARTESIAN_POINT('',(0.999999342796208,0.00487121530971084,8.80019806641107));
#8822=CARTESIAN_POINT('Origin',(1.,0.,8.86));
#8823=CARTESIAN_POINT('',(1.00430619197361,-0.00485923077359697,11.9996476704237));
#8824=CARTESIAN_POINT('Ctrl Pts',(0.999999342796208,0.0048712153097108,
8.80019806641107));
#8825=CARTESIAN_POINT('Ctrl Pts',(0.99996896462742,0.230035163961994,8.81853897995701));
#8826=CARTESIAN_POINT('Ctrl Pts',(0.843216945008081,0.678245689353448,8.85526000727444));
#8827=CARTESIAN_POINT('Ctrl Pts',(0.23714388778331,1.05999084182087,8.91053070559157));
#8828=CARTESIAN_POINT('Ctrl Pts',(-0.476746387578999,0.979670338171269,
8.96597705173729));
#8829=CARTESIAN_POINT('Ctrl Pts',(-0.98657616663209,0.470389879273211,9.0216024298575));
#8830=CARTESIAN_POINT('Ctrl Pts',(-1.06798165663575,-0.248000588468906,
9.07740270249169));
#8831=CARTESIAN_POINT('Ctrl Pts',(-0.682243081073035,-0.862304425765768,
9.1333764236107));
#8832=CARTESIAN_POINT('Ctrl Pts',(-0.196330490445415,-1.03251494397982,
9.17314484390509));
#8833=CARTESIAN_POINT('Ctrl Pts',(0.0904960552365201,-1.02015022040365,
9.19657718102618));
#8834=CARTESIAN_POINT('Ctrl Pts',(0.204441911777542,-1.00572651008441,9.20595357869542));
#8835=CARTESIAN_POINT('Ctrl Pts',(0.343951015893895,-0.96975630344906,9.21768054548145));
#8836=CARTESIAN_POINT('Ctrl Pts',(0.501773879908335,-0.899045416054097,
9.23176320323934));
#8837=CARTESIAN_POINT('Ctrl Pts',(0.768592409823833,-0.721243151610969,
9.2578611494339));
#8838=CARTESIAN_POINT('Ctrl Pts',(1.04382114359922,-0.318042243912805,9.29602676229045));
#8839=CARTESIAN_POINT('Ctrl Pts',(1.04456490155922,0.326294295864951,9.34634267499162));
#8840=CARTESIAN_POINT('Ctrl Pts',(0.711307557250243,0.815326125223123,9.39257751006242));
#8841=CARTESIAN_POINT('Ctrl Pts',(0.234442425347365,1.04427973165066,9.43469552996756));
#8842=CARTESIAN_POINT('Ctrl Pts',(-0.242097506080382,1.04460426316974,9.47266669612882));
#8843=CARTESIAN_POINT('Ctrl Pts',(-0.672296189994615,0.837312084419627,
9.51070107270169));
#8844=CARTESIAN_POINT('Ctrl Pts',(-0.970493141256397,0.463551157181226,
9.54879683116503));
#8845=CARTESIAN_POINT('Ctrl Pts',(-1.07723336834064,-0.00342794058422688,
9.58695206272228));
#8846=CARTESIAN_POINT('Ctrl Pts',(-0.988260429843343,-0.39307851175747,
9.61879599421848));
#8847=CARTESIAN_POINT('Ctrl Pts',(-0.82093539560644,-0.658946730224756,
9.64429884892662));
#8848=CARTESIAN_POINT('Ctrl Pts',(-0.598840710302034,-0.88141322392247,
9.66981982299092));
#8849=CARTESIAN_POINT('Ctrl Pts',(-0.237756057923814,-1.05547919442497,
9.70175433946707));
#8850=CARTESIAN_POINT('Ctrl Pts',(0.243905786180905,-1.05553040152794,9.74012683420727));
#8851=CARTESIAN_POINT('Ctrl Pts',(0.678604028637572,-0.846341399380819,
9.77854812145871));
#8852=CARTESIAN_POINT('Ctrl Pts',(0.979430107833126,-0.468912235308927,
9.81701586224876));
#8853=CARTESIAN_POINT('Ctrl Pts',(1.09985901046267,0.0548445677701001,9.85980673545165));
#8854=CARTESIAN_POINT('Ctrl Pts',(0.921933505746503,0.631124795915794,9.90693599171239));
#8855=CARTESIAN_POINT('Ctrl Pts',(0.4929126040201,0.973793160670524,9.94983738646297));
#8856=CARTESIAN_POINT('Ctrl Pts',(0.0780904371091028,1.06751269479759,9.98418939216924));
#8857=CARTESIAN_POINT('Ctrl Pts',(-0.346188348797786,1.0365452542535,10.0185609429505));
#8858=CARTESIAN_POINT('Ctrl Pts',(-0.822968443953264,0.76162232341949,10.0615600576428));
#8859=CARTESIAN_POINT('Ctrl Pts',(-1.11011929233597,0.166104281872854,10.1132080400722));
#8860=CARTESIAN_POINT('Ctrl Pts',(-1.0081246602054,-0.515708350877839,10.1670522944212));
#8861=CARTESIAN_POINT('Ctrl Pts',(-0.494775946618556,-1.02970801548153,
10.2230915794475));
#8862=CARTESIAN_POINT('Ctrl Pts',(0.171330015334639,-1.10394798748412,10.2748519542969));
#8863=CARTESIAN_POINT('Ctrl Pts',(0.683814393710209,-0.85633240678914,10.3201591760856));
#8864=CARTESIAN_POINT('Ctrl Pts',(0.987375224349673,-0.475369257557772,
10.3590026286433));
#8865=CARTESIAN_POINT('Ctrl Pts',(1.11501021817459,0.0796008030233853,10.4043267361272));
#8866=CARTESIAN_POINT('Ctrl Pts',(0.894257942603671,0.712772351603783,10.4561304980607));
#8867=CARTESIAN_POINT('Ctrl Pts',(0.254526418580225,1.11465334671006,10.5144063331842));
#8868=CARTESIAN_POINT('Ctrl Pts',(-0.495386650979013,1.03000796421648,10.5726689321936));
#8869=CARTESIAN_POINT('Ctrl Pts',(-1.02902006816757,0.496451864872819,10.6309084916996));
#8870=CARTESIAN_POINT('Ctrl Pts',(-1.11329107431628,-0.25302544687232,10.6891152782939));
#8871=CARTESIAN_POINT('Ctrl Pts',(-0.712411475504087,-0.890954531307481,
10.7472796615617));
#8872=CARTESIAN_POINT('Ctrl Pts',(-0.00144545535703713,-1.13970545531556,
10.8053921361455));
#8873=CARTESIAN_POINT('Ctrl Pts',(0.589562318042014,-0.932130645422847,
10.8537681412278));
#8874=CARTESIAN_POINT('Ctrl Pts',(0.908494555547074,-0.573322783618425,
10.8924337348326));
#8875=CARTESIAN_POINT('Ctrl Pts',(1.0932000203843,-0.130460109720627,10.9310743576345));
#8876=CARTESIAN_POINT('Ctrl Pts',(1.02452819258886,0.49024714203063,10.9793255246093));
#8877=CARTESIAN_POINT('Ctrl Pts',(0.493612168598575,1.02033558321459,11.037138824411));
#8878=CARTESIAN_POINT('Ctrl Pts',(-0.166230575259128,1.09368100121347,11.0884425957329));
#8879=CARTESIAN_POINT('Ctrl Pts',(-0.673140522140151,0.84850197959383,11.1332655331794));
#8880=CARTESIAN_POINT('Ctrl Pts',(-0.973483979429893,0.47222295927322,11.1716363210045));
#8881=CARTESIAN_POINT('Ctrl Pts',(-1.08028898641827,0.00311472479435195,
11.2099559586628));
#8882=CARTESIAN_POINT('Ctrl Pts',(-0.973354083483389,-0.465125791076451,
11.2482222395404));
#8883=CARTESIAN_POINT('Ctrl Pts',(-0.674252322492463,-0.840091585392608,
11.2864330284043));
#8884=CARTESIAN_POINT('Ctrl Pts',(-0.242715089956039,-1.04789098180051,
11.3245862592493));
#8885=CARTESIAN_POINT('Ctrl Pts',(0.23542767696283,-1.04765866302507,11.3626799542613));
#8886=CARTESIAN_POINT('Ctrl Pts',(0.665536159094464,-0.840435751119737,
11.4007121983223));
#8887=CARTESIAN_POINT('Ctrl Pts',(0.962591820228485,-0.467820172164233,
11.4386811727585));
#8888=CARTESIAN_POINT('Ctrl Pts',(1.06846208937938,-0.00379118886353965,
11.47658513569));
#8889=CARTESIAN_POINT('Ctrl Pts',(0.962501175338684,0.458913289962351,11.5144224357756));
#8890=CARTESIAN_POINT('Ctrl Pts',(0.618041205754224,0.892154566858533,11.5584863515166));
#8891=CARTESIAN_POINT('Ctrl Pts',(0.00421838652791971,1.10738146763147,
11.6087289304493));
#8892=CARTESIAN_POINT('Ctrl Pts',(-0.685284502455283,0.86560690604705,11.6650903417562));
#8893=CARTESIAN_POINT('Ctrl Pts',(-1.07219887432344,0.249028474249683,11.7212863124465));
#8894=CARTESIAN_POINT('Ctrl Pts',(-0.990640181337795,-0.472396051339649,
11.7773128627812));
#8895=CARTESIAN_POINT('Ctrl Pts',(-0.478640001005609,-0.983760746265736,
11.8331676524783));
#8896=CARTESIAN_POINT('Ctrl Pts',(0.238202676882345,-1.06445286799178,11.8888462567429));
#8897=CARTESIAN_POINT('Ctrl Pts',(0.846858663881909,-0.681098479204223,
11.9443505326692));
#8898=CARTESIAN_POINT('Ctrl Pts',(1.00427568511571,-0.230977292777482,11.9812290386622));
#8899=CARTESIAN_POINT('Ctrl Pts',(1.00430619197361,-0.004859230773597,11.9996476704237));
#8900=CARTESIAN_POINT('Origin',(1.,-1.33226762955019E-15,11.94));
#8901=CARTESIAN_POINT('Origin',(1.,-1.33226762955019E-15,11.94));
#8902=CARTESIAN_POINT('Origin',(1.,0.,8.86));
#8903=CARTESIAN_POINT('',(0.,0.,0.));
#8904=CARTESIAN_POINT('Origin',(-4.,-3.,-0.1));
#8905=CARTESIAN_POINT('',(-4.21,-3.,0.));
#8906=CARTESIAN_POINT('Origin',(-4.,-3.,0.));
#8907=CARTESIAN_POINT('',(-4.21,-3.,1.1));
#8908=CARTESIAN_POINT('',(-4.21,-3.,-0.1));
#8909=CARTESIAN_POINT('Origin',(-4.,-3.,1.1));
#8910=CARTESIAN_POINT('Origin',(-4.,-3.,1.1));
#8911=CARTESIAN_POINT('Origin',(0.,-1.55,16.));
#8912=CARTESIAN_POINT('',(-3.5,-2.5,16.));
#8913=CARTESIAN_POINT('',(-3.5,-3.5,16.));
#8914=CARTESIAN_POINT('',(-3.5,-2.525,16.));
#8915=CARTESIAN_POINT('',(-4.5,-2.5,16.));
#8916=CARTESIAN_POINT('',(-1.75,-2.5,16.));
#8917=CARTESIAN_POINT('',(-4.5,0.4,16.));
#8918=CARTESIAN_POINT('',(-4.5,0.4,16.));
#8919=CARTESIAN_POINT('',(4.5,0.4,16.));
#8920=CARTESIAN_POINT('',(4.5,0.4,16.));
#8921=CARTESIAN_POINT('',(4.5,-3.5,16.));
#8922=CARTESIAN_POINT('',(4.5,-3.5,16.));
#8923=CARTESIAN_POINT('',(-4.5,-3.5,16.));
#8924=CARTESIAN_POINT('Origin',(4.5,0.4,16.));
#8925=CARTESIAN_POINT('',(-4.5,0.4,16.5));
#8926=CARTESIAN_POINT('',(-4.5,0.4,16.));
#8927=CARTESIAN_POINT('',(4.5,0.4,16.5));
#8928=CARTESIAN_POINT('',(4.5,0.4,16.5));
#8929=CARTESIAN_POINT('',(4.5,0.4,16.));
#8930=CARTESIAN_POINT('Origin',(4.5,-3.5,16.));
#8931=CARTESIAN_POINT('',(4.5,-3.5,16.5));
#8932=CARTESIAN_POINT('',(4.5,-3.5,16.5));
#8933=CARTESIAN_POINT('',(4.5,-3.5,16.));
#8934=CARTESIAN_POINT('Origin',(-4.5,-3.5,0.));
#8935=CARTESIAN_POINT('',(-4.5,-3.5,0.));
#8936=CARTESIAN_POINT('',(-4.5,-3.5,16.5));
#8937=CARTESIAN_POINT('',(-4.5,-3.5,0.));
#8938=CARTESIAN_POINT('',(-3.5,-3.5,0.));
#8939=CARTESIAN_POINT('',(-4.5,-3.5,0.));
#8940=CARTESIAN_POINT('',(-3.5,-3.5,0.));
#8941=CARTESIAN_POINT('',(-4.5,-3.5,16.5));
#8942=CARTESIAN_POINT('Origin',(-4.5,-2.5,0.));
#8943=CARTESIAN_POINT('',(-4.5,-2.5,0.));
#8944=CARTESIAN_POINT('',(-4.5,-2.5,0.));
#8945=CARTESIAN_POINT('',(-4.5,-2.5,0.));
#8946=CARTESIAN_POINT('',(-4.5,0.4,16.5));
#8947=CARTESIAN_POINT('Origin',(-3.5,-2.5,0.));
#8948=CARTESIAN_POINT('',(-3.5,-2.5,0.));
#8949=CARTESIAN_POINT('',(-3.5,-2.5,0.));
#8950=CARTESIAN_POINT('',(-3.5,-2.5,0.));
#8951=CARTESIAN_POINT('Origin',(-3.5,-3.5,0.));
#8952=CARTESIAN_POINT('',(-3.5,-3.5,0.));
#8953=CARTESIAN_POINT('Origin',(-4.,-3.,16.5));
#8954=CARTESIAN_POINT('Origin',(-4.,-3.,0.));
#8955=CARTESIAN_POINT('',(0.,0.,0.));
#8956=CARTESIAN_POINT('Origin',(4.,6.,1.2));
#8957=CARTESIAN_POINT('',(3.2,6.,1.2));
#8958=CARTESIAN_POINT('',(3.2,6.26274169979695,1.2));
#8959=CARTESIAN_POINT('',(3.2,6.,1.2));
#8960=CARTESIAN_POINT('',(4.,6.,2.));
#8961=CARTESIAN_POINT('Origin',(4.,6.,1.2));
#8962=CARTESIAN_POINT('',(4.,6.4,2.));
#8963=CARTESIAN_POINT('',(4.,6.,2.));
#8964=CARTESIAN_POINT('Ctrl Pts',(3.2,6.26274169979695,1.2));
#8965=CARTESIAN_POINT('Ctrl Pts',(3.2,6.26274169979695,1.09868315167368));
#8966=CARTESIAN_POINT('Ctrl Pts',(3.22040772858495,6.270261426297,0.991198421229182));
#8967=CARTESIAN_POINT('Ctrl Pts',(3.30227767389892,6.29674433020986,0.794357456033841));
#8968=CARTESIAN_POINT('Ctrl Pts',(3.36370361600024,6.31525508485039,0.704925534101287));
#8969=CARTESIAN_POINT('Ctrl Pts',(3.50489278468399,6.34949848812546,0.563736365417532));
#8970=CARTESIAN_POINT('Ctrl Pts',(3.59433775043408,6.36754956424272,0.502285211106731));
#8971=CARTESIAN_POINT('Ctrl Pts',(3.79122709022331,6.39296190354765,0.420396463357562));
#8972=CARTESIAN_POINT('Ctrl Pts',(3.89873014250612,6.4,0.4));
#8973=CARTESIAN_POINT('Ctrl Pts',(4.10126985749388,6.4,0.4));
#8974=CARTESIAN_POINT('Ctrl Pts',(4.20877290977669,6.39296190354765,0.420396463357562));
#8975=CARTESIAN_POINT('Ctrl Pts',(4.40566224956592,6.36754956424272,0.502285211106731));
#8976=CARTESIAN_POINT('Ctrl Pts',(4.49510721531601,6.34949848812546,0.563736365417532));
#8977=CARTESIAN_POINT('Ctrl Pts',(4.63629638399976,6.31525508485039,0.704925534101287));
#8978=CARTESIAN_POINT('Ctrl Pts',(4.69772232610108,6.29674433020986,0.794357456033842));
#8979=CARTESIAN_POINT('Ctrl Pts',(4.77959227141505,6.270261426297,0.991198421229182));
#8980=CARTESIAN_POINT('Ctrl Pts',(4.8,6.26274169979695,1.09868315167368));
#8981=CARTESIAN_POINT('Ctrl Pts',(4.8,6.26274169979695,1.30131684832632));
#8982=CARTESIAN_POINT('Ctrl Pts',(4.77959227141505,6.270261426297,1.40880157877082));
#8983=CARTESIAN_POINT('Ctrl Pts',(4.69772232610108,6.29674433020986,1.60564254396616));
#8984=CARTESIAN_POINT('Ctrl Pts',(4.63629638399976,6.31525508485039,1.69507446589871));
#8985=CARTESIAN_POINT('Ctrl Pts',(4.49510721531601,6.34949848812546,1.83626363458247));
#8986=CARTESIAN_POINT('Ctrl Pts',(4.40566224956592,6.36754956424272,1.89771478889327));
#8987=CARTESIAN_POINT('Ctrl Pts',(4.20877290977668,6.39296190354765,1.97960353664244));
#8988=CARTESIAN_POINT('Ctrl Pts',(4.10126985749388,6.4,2.));
#8989=CARTESIAN_POINT('Ctrl Pts',(4.,6.4,2.));
#8990=CARTESIAN_POINT('Origin',(4.,4.5,1.2));
#8991=CARTESIAN_POINT('',(4.2,4.5,1.2));
#8992=CARTESIAN_POINT('',(3.8,4.5,1.2));
#8993=CARTESIAN_POINT('',(4.,4.5,1.2));
#8994=CARTESIAN_POINT('Origin',(4.,4.5,1.2));
#8995=CARTESIAN_POINT('Origin',(4.,4.5,1.2));
#8996=CARTESIAN_POINT('',(4.2,4.97979589711327,1.2));
#8997=CARTESIAN_POINT('',(4.2,4.5,1.2));
#8998=CARTESIAN_POINT('',(3.8,4.97979589711327,1.2));
#8999=CARTESIAN_POINT('Ctrl Pts',(3.8,4.97979589711327,1.2));
#9000=CARTESIAN_POINT('Ctrl Pts',(3.8,4.97979589711327,1.22518635039268));
#9001=CARTESIAN_POINT('Ctrl Pts',(3.80504744075028,4.98086775323689,1.25200355543238));
#9002=CARTESIAN_POINT('Ctrl Pts',(3.82547891647032,4.98470830158554,1.30125840100601));
#9003=CARTESIAN_POINT('Ctrl Pts',(3.84085937956158,4.98741817020387,1.3237020920362));
#9004=CARTESIAN_POINT('Ctrl Pts',(3.87629691507098,4.99248067527664,1.3591396275456));
#9005=CARTESIAN_POINT('Ctrl Pts',(3.89874102776047,4.99516669430373,1.37452086830895));
#9006=CARTESIAN_POINT('Ctrl Pts',(3.94799733878363,4.99895237729416,1.39495290844717));
#9007=CARTESIAN_POINT('Ctrl Pts',(3.97481506091572,5.,1.4));
#9008=CARTESIAN_POINT('Ctrl Pts',(4.02518493908428,5.,1.4));
#9009=CARTESIAN_POINT('Ctrl Pts',(4.05200266121637,4.99895237729416,1.39495290844717));
#9010=CARTESIAN_POINT('Ctrl Pts',(4.10125897223952,4.99516669430373,1.37452086830895));
#9011=CARTESIAN_POINT('Ctrl Pts',(4.12370308492902,4.99248067527664,1.3591396275456));
#9012=CARTESIAN_POINT('Ctrl Pts',(4.15914062043842,4.98741817020387,1.3237020920362));
#9013=CARTESIAN_POINT('Ctrl Pts',(4.17452108352968,4.98470830158554,1.30125840100601));
#9014=CARTESIAN_POINT('Ctrl Pts',(4.19495255924972,4.98086775323689,1.25200355543238));
#9015=CARTESIAN_POINT('Ctrl Pts',(4.2,4.97979589711327,1.22518635039268));
#9016=CARTESIAN_POINT('Ctrl Pts',(4.2,4.97979589711327,1.2));
#9017=CARTESIAN_POINT('',(3.8,5.35,1.2));
#9018=CARTESIAN_POINT('',(3.8,4.5,1.2));
#9019=CARTESIAN_POINT('Origin',(4.,5.35,1.2));
#9020=CARTESIAN_POINT('',(3.8,4.5,1.2));
#9021=CARTESIAN_POINT('Origin',(4.,4.,1.2));
#9022=CARTESIAN_POINT('',(3.,4.,1.2));
#9023=CARTESIAN_POINT('Origin',(4.,4.,1.2));
#9024=CARTESIAN_POINT('Origin',(4.,4.,1.2));
#9025=CARTESIAN_POINT('Origin',(4.,5.35,1.2));
#9026=CARTESIAN_POINT('',(3.485,5.35,1.2));
#9027=CARTESIAN_POINT('Origin',(4.,5.35,1.2));
#9028=CARTESIAN_POINT('',(3.485,6.,1.2));
#9029=CARTESIAN_POINT('',(3.485,5.35,1.2));
#9030=CARTESIAN_POINT('Origin',(4.,6.,1.2));
#9031=CARTESIAN_POINT('Origin',(4.,5.35,1.2));
#9032=CARTESIAN_POINT('Origin',(4.,6.,1.2));
#9033=CARTESIAN_POINT('Ctrl Pts',(4.,6.4,2.));
#9034=CARTESIAN_POINT('Ctrl Pts',(3.89873014250612,6.4,2.));
#9035=CARTESIAN_POINT('Ctrl Pts',(3.79122709022331,6.39296190354765,1.97960353664244));
#9036=CARTESIAN_POINT('Ctrl Pts',(3.59433775043408,6.36754956424272,1.89771478889327));
#9037=CARTESIAN_POINT('Ctrl Pts',(3.50489278468399,6.34949848812546,1.83626363458247));
#9038=CARTESIAN_POINT('Ctrl Pts',(3.36370361600024,6.31525508485039,1.69507446589871));
#9039=CARTESIAN_POINT('Ctrl Pts',(3.30227767389892,6.29674433020986,1.60564254396616));
#9040=CARTESIAN_POINT('Ctrl Pts',(3.22040772858495,6.270261426297,1.40880157877082));
#9041=CARTESIAN_POINT('Ctrl Pts',(3.2,6.26274169979695,1.30131684832632));
#9042=CARTESIAN_POINT('Ctrl Pts',(3.2,6.26274169979695,1.2));
#9043=CARTESIAN_POINT('',(4.,6.,2.));
#9044=CARTESIAN_POINT('Origin',(4.,6.,1.2));
#9045=CARTESIAN_POINT('Origin',(4.,6.,1.2));
#9046=CARTESIAN_POINT('Origin',(4.,4.,0.));
#9047=CARTESIAN_POINT('',(1.6,4.,2.));
#9048=CARTESIAN_POINT('Origin',(4.,4.,2.));
#9049=CARTESIAN_POINT('Origin',(4.,4.,2.));
#9050=CARTESIAN_POINT('',(1.6,4.,0.));
#9051=CARTESIAN_POINT('',(1.6,4.,0.));
#9052=CARTESIAN_POINT('Origin',(4.,4.,0.));
#9053=CARTESIAN_POINT('Origin',(4.,4.,1.9));
#9054=CARTESIAN_POINT('',(2.75,4.,1.9));
#9055=CARTESIAN_POINT('Origin',(4.,4.,1.9));
#9056=CARTESIAN_POINT('',(2.75,4.,2.));
#9057=CARTESIAN_POINT('',(2.75,4.,1.9));
#9058=CARTESIAN_POINT('Origin',(4.,4.,2.));
#9059=CARTESIAN_POINT('Origin',(4.,4.,1.9));
#9060=CARTESIAN_POINT('',(3.,4.,1.9));
#9061=CARTESIAN_POINT('Origin',(4.,4.,1.9));
#9062=CARTESIAN_POINT('Origin',(4.,4.,1.2));
#9063=CARTESIAN_POINT('',(3.,4.,1.2));
#9064=CARTESIAN_POINT('Origin',(2.72720779386421,2.72720779386421,-0.1));
#9065=CARTESIAN_POINT('',(2.45220779386421,2.72720779386421,0.));
#9066=CARTESIAN_POINT('Origin',(2.72720779386421,2.72720779386421,0.));
#9067=CARTESIAN_POINT('',(2.45220779386421,2.72720779386421,2.));
#9068=CARTESIAN_POINT('',(2.45220779386421,2.72720779386421,-0.1));
#9069=CARTESIAN_POINT('Origin',(2.72720779386421,2.72720779386421,2.));
#9070=CARTESIAN_POINT('Origin',(2.72720779386421,5.27279220613579,-0.1));
#9071=CARTESIAN_POINT('',(2.45220779386421,5.27279220613579,0.));
#9072=CARTESIAN_POINT('Origin',(2.72720779386421,5.27279220613579,0.));
#9073=CARTESIAN_POINT('',(2.45220779386421,5.27279220613579,2.));
#9074=CARTESIAN_POINT('',(2.45220779386421,5.27279220613579,-0.1));
#9075=CARTESIAN_POINT('Origin',(2.72720779386421,5.27279220613579,2.));
#9076=CARTESIAN_POINT('Origin',(5.27279220613579,5.27279220613579,-0.1));
#9077=CARTESIAN_POINT('',(4.99779220613579,5.27279220613579,0.));
#9078=CARTESIAN_POINT('Origin',(5.27279220613579,5.27279220613579,0.));
#9079=CARTESIAN_POINT('',(4.99779220613579,5.27279220613579,2.));
#9080=CARTESIAN_POINT('',(4.99779220613579,5.27279220613579,-0.1));
#9081=CARTESIAN_POINT('Origin',(5.27279220613579,5.27279220613579,2.));
#9082=CARTESIAN_POINT('Origin',(5.27279220613578,2.72720779386421,-0.1));
#9083=CARTESIAN_POINT('',(4.99779220613578,2.72720779386421,0.));
#9084=CARTESIAN_POINT('Origin',(5.27279220613578,2.72720779386421,0.));
#9085=CARTESIAN_POINT('',(4.99779220613578,2.72720779386421,2.));
#9086=CARTESIAN_POINT('',(4.99779220613578,2.72720779386421,-0.1));
#9087=CARTESIAN_POINT('Origin',(5.27279220613578,2.72720779386421,2.));
#9088=CARTESIAN_POINT('Origin',(4.,4.,2.));
#9089=CARTESIAN_POINT('Origin',(4.,4.,0.));
#9090=CARTESIAN_POINT('',(0.,0.,0.));
#9091=CARTESIAN_POINT('Origin',(4.,4.,1.9));
#9092=CARTESIAN_POINT('',(3.,4.,2.));
#9093=CARTESIAN_POINT('Origin',(4.,4.,2.));
#9094=CARTESIAN_POINT('',(3.,4.,1.9));
#9095=CARTESIAN_POINT('',(3.,4.,1.9));
#9096=CARTESIAN_POINT('Origin',(4.,4.,1.9));
#9097=CARTESIAN_POINT('Origin',(4.,4.,1.9));
#9098=CARTESIAN_POINT('',(2.75,4.,2.));
#9099=CARTESIAN_POINT('Origin',(4.,4.,2.));
#9100=CARTESIAN_POINT('',(2.75,4.,1.9));
#9101=CARTESIAN_POINT('',(2.75,4.,1.9));
#9102=CARTESIAN_POINT('Origin',(4.,4.,1.9));
#9103=CARTESIAN_POINT('Origin',(4.,4.,2.));
#9104=CARTESIAN_POINT('Origin',(4.,4.,1.9));
#9105=CARTESIAN_POINT('',(0.,0.,0.));
#9106=CARTESIAN_POINT('Origin',(4.,4.6,9.1));
#9107=CARTESIAN_POINT('',(4.11180339887499,4.5,9.1));
#9108=CARTESIAN_POINT('',(3.88819660112501,4.5,9.1));
#9109=CARTESIAN_POINT('',(4.,4.5,9.1));
#9110=CARTESIAN_POINT('Origin',(4.,4.6,9.1));
#9111=CARTESIAN_POINT('Origin',(4.,4.6,8.4));
#9112=CARTESIAN_POINT('',(3.85,4.6,8.5));
#9113=CARTESIAN_POINT('Origin',(4.,4.6,8.5));
#9114=CARTESIAN_POINT('',(3.85,4.6,8.86771243444677));
#9115=CARTESIAN_POINT('',(3.85,4.6,8.4));
#9116=CARTESIAN_POINT('',(3.88819660112501,4.5,8.83416876048223));
#9117=CARTESIAN_POINT('Ctrl Pts',(3.88819660112501,4.5,8.83416876048223));
#9118=CARTESIAN_POINT('Ctrl Pts',(3.87757657209989,4.5118735534116,8.84132878259032));
#9119=CARTESIAN_POINT('Ctrl Pts',(3.86846014424429,4.52597563413084,8.84907123479525));
#9120=CARTESIAN_POINT('Ctrl Pts',(3.85804355837321,4.55054285102637,8.85901486480765));
#9121=CARTESIAN_POINT('Ctrl Pts',(3.8550467625566,4.56012752110791,8.86217045472001));
#9122=CARTESIAN_POINT('Ctrl Pts',(3.85102541664982,4.57981886189345,8.86652445682054));
#9123=CARTESIAN_POINT('Ctrl Pts',(3.85,4.58992766139246,8.86771243444677));
#9124=CARTESIAN_POINT('Ctrl Pts',(3.85,4.6,8.86771243444677));
#9125=CARTESIAN_POINT('',(3.88819660112501,4.5,8.4));
#9126=CARTESIAN_POINT('',(4.11180339887499,4.5,8.83416876048223));
#9127=CARTESIAN_POINT('',(4.11180339887499,4.5,8.4));
#9128=CARTESIAN_POINT('Ctrl Pts',(3.85,4.6,8.86771243444677));
#9129=CARTESIAN_POINT('Ctrl Pts',(3.85,4.61007233860753,8.86771243444677));
#9130=CARTESIAN_POINT('Ctrl Pts',(3.85102541664981,4.62018113810654,8.86652445682054));
#9131=CARTESIAN_POINT('Ctrl Pts',(3.85504676255659,4.63987247889209,8.86217045472001));
#9132=CARTESIAN_POINT('Ctrl Pts',(3.85804355837321,4.64945714897362,8.85901486480765));
#9133=CARTESIAN_POINT('Ctrl Pts',(3.8696156276414,4.67674954008529,8.84796821509873));
#9134=CARTESIAN_POINT('Ctrl Pts',(3.88090702862397,4.69303906297994,8.83859067358653));
#9135=CARTESIAN_POINT('Ctrl Pts',(3.90668694057098,4.71881897492694,8.82246422388431));
#9136=CARTESIAN_POINT('Ctrl Pts',(3.9230088222236,4.73027430044143,8.81441378257927));
#9137=CARTESIAN_POINT('Ctrl Pts',(3.95978537347009,4.74588290014714,8.80314301976006));
#9138=CARTESIAN_POINT('Ctrl Pts',(3.98027902658713,4.75,8.8));
#9139=CARTESIAN_POINT('Ctrl Pts',(4.01972097341287,4.75,8.8));
#9140=CARTESIAN_POINT('Ctrl Pts',(4.04021462652991,4.74588290014714,8.80314301976006));
#9141=CARTESIAN_POINT('Ctrl Pts',(4.0769911777764,4.73027430044143,8.81441378257927));
#9142=CARTESIAN_POINT('Ctrl Pts',(4.09331305942902,4.71881897492694,8.82246422388431));
#9143=CARTESIAN_POINT('Ctrl Pts',(4.11909297137603,4.69303906297994,8.83859067358653));
#9144=CARTESIAN_POINT('Ctrl Pts',(4.1303843723586,4.67674954008529,8.84796821509873));
#9145=CARTESIAN_POINT('Ctrl Pts',(4.14195644162679,4.64945714897363,8.85901486480765));
#9146=CARTESIAN_POINT('Ctrl Pts',(4.1449532374434,4.63987247889209,8.86217045472001));
#9147=CARTESIAN_POINT('Ctrl Pts',(4.14897458335018,4.62018113810655,8.86652445682054));
#9148=CARTESIAN_POINT('Ctrl Pts',(4.15,4.61007233860753,8.86771243444677));
#9149=CARTESIAN_POINT('Ctrl Pts',(4.15,4.6,8.86771243444677));
#9150=CARTESIAN_POINT('Ctrl Pts',(4.15,4.58992766139246,8.86771243444677));
#9151=CARTESIAN_POINT('Ctrl Pts',(4.14897458335018,4.57981886189345,8.86652445682054));
#9152=CARTESIAN_POINT('Ctrl Pts',(4.1449532374434,4.56012752110791,8.86217045472001));
#9153=CARTESIAN_POINT('Ctrl Pts',(4.14195644162679,4.55054285102637,8.85901486480765));
#9154=CARTESIAN_POINT('Ctrl Pts',(4.13153985575571,4.52597563413084,8.84907123479525));
#9155=CARTESIAN_POINT('Ctrl Pts',(4.12242342790011,4.5118735534116,8.84132878259032));
#9156=CARTESIAN_POINT('Ctrl Pts',(4.11180339887499,4.5,8.83416876048223));
#9157=CARTESIAN_POINT('Origin',(4.,4.5,9.));
#9158=CARTESIAN_POINT('',(3.8,4.5,9.));
#9159=CARTESIAN_POINT('Origin',(4.,4.5,9.));
#9160=CARTESIAN_POINT('Origin',(4.,4.5,9.));
#9161=CARTESIAN_POINT('Origin',(4.,4.5,9.));
#9162=CARTESIAN_POINT('',(3.8,5.35,9.));
#9163=CARTESIAN_POINT('',(3.8,4.5,9.));
#9164=CARTESIAN_POINT('Origin',(4.,5.35,9.));
#9165=CARTESIAN_POINT('Origin',(4.,5.35,9.));
#9166=CARTESIAN_POINT('',(3.485,5.35,9.));
#9167=CARTESIAN_POINT('Origin',(4.,5.35,9.));
#9168=CARTESIAN_POINT('',(3.485,6.,9.));
#9169=CARTESIAN_POINT('',(3.485,5.35,9.));
#9170=CARTESIAN_POINT('Origin',(4.,6.,9.));
#9171=CARTESIAN_POINT('Origin',(4.,5.35,9.));
#9172=CARTESIAN_POINT('Origin',(4.,6.,9.));
#9173=CARTESIAN_POINT('',(3.2,6.,9.));
#9174=CARTESIAN_POINT('Origin',(4.,6.,9.));
#9175=CARTESIAN_POINT('',(3.2,6.26274169979695,9.));
#9176=CARTESIAN_POINT('',(3.2,6.,9.));
#9177=CARTESIAN_POINT('Ctrl Pts',(3.2,6.26274169979695,9.));
#9178=CARTESIAN_POINT('Ctrl Pts',(3.2,6.26274169979695,8.89868315167368));
#9179=CARTESIAN_POINT('Ctrl Pts',(3.22040772858495,6.270261426297,8.79119842122918));
#9180=CARTESIAN_POINT('Ctrl Pts',(3.30227767389892,6.29674433020986,8.59435745603384));
#9181=CARTESIAN_POINT('Ctrl Pts',(3.36370361600024,6.31525508485039,8.50492553410129));
#9182=CARTESIAN_POINT('Ctrl Pts',(3.50489278468399,6.34949848812546,8.36373636541753));
#9183=CARTESIAN_POINT('Ctrl Pts',(3.59433775043408,6.36754956424272,8.30228521110673));
#9184=CARTESIAN_POINT('Ctrl Pts',(3.79122709022331,6.39296190354765,8.22039646335756));
#9185=CARTESIAN_POINT('Ctrl Pts',(3.89873014250612,6.4,8.2));
#9186=CARTESIAN_POINT('Ctrl Pts',(4.10126985749388,6.4,8.2));
#9187=CARTESIAN_POINT('Ctrl Pts',(4.20877290977668,6.39296190354765,8.22039646335756));
#9188=CARTESIAN_POINT('Ctrl Pts',(4.40566224956592,6.36754956424272,8.30228521110673));
#9189=CARTESIAN_POINT('Ctrl Pts',(4.49510721531601,6.34949848812546,8.36373636541753));
#9190=CARTESIAN_POINT('Ctrl Pts',(4.63629638399976,6.31525508485039,8.50492553410129));
#9191=CARTESIAN_POINT('Ctrl Pts',(4.69772232610108,6.29674433020987,8.59435745603384));
#9192=CARTESIAN_POINT('Ctrl Pts',(4.77959227141505,6.270261426297,8.79119842122918));
#9193=CARTESIAN_POINT('Ctrl Pts',(4.8,6.26274169979695,8.89868315167368));
#9194=CARTESIAN_POINT('Ctrl Pts',(4.8,6.26274169979695,9.10131684832632));
#9195=CARTESIAN_POINT('Ctrl Pts',(4.77959227141505,6.270261426297,9.20880157877082));
#9196=CARTESIAN_POINT('Ctrl Pts',(4.69772232610108,6.29674433020986,9.40564254396616));
#9197=CARTESIAN_POINT('Ctrl Pts',(4.63629638399976,6.31525508485039,9.49507446589871));
#9198=CARTESIAN_POINT('Ctrl Pts',(4.49510721531601,6.34949848812546,9.63626363458247));
#9199=CARTESIAN_POINT('Ctrl Pts',(4.40566224956592,6.36754956424272,9.69771478889327));
#9200=CARTESIAN_POINT('Ctrl Pts',(4.20877290977668,6.39296190354765,9.77960353664244));
#9201=CARTESIAN_POINT('Ctrl Pts',(4.10126985749388,6.4,9.8));
#9202=CARTESIAN_POINT('Ctrl Pts',(3.89873014250612,6.4,9.8));
#9203=CARTESIAN_POINT('Ctrl Pts',(3.79122709022331,6.39296190354765,9.77960353664244));
#9204=CARTESIAN_POINT('Ctrl Pts',(3.59433775043408,6.36754956424272,9.69771478889327));
#9205=CARTESIAN_POINT('Ctrl Pts',(3.50489278468399,6.34949848812546,9.63626363458247));
#9206=CARTESIAN_POINT('Ctrl Pts',(3.36370361600024,6.31525508485039,9.49507446589871));
#9207=CARTESIAN_POINT('Ctrl Pts',(3.30227767389892,6.29674433020986,9.40564254396616));
#9208=CARTESIAN_POINT('Ctrl Pts',(3.22040772858495,6.270261426297,9.20880157877082));
#9209=CARTESIAN_POINT('Ctrl Pts',(3.2,6.26274169979695,9.10131684832632));
#9210=CARTESIAN_POINT('Ctrl Pts',(3.2,6.26274169979695,9.));
#9211=CARTESIAN_POINT('Origin',(4.,6.,9.));
#9212=CARTESIAN_POINT('Origin',(4.,4.,9.4));
#9213=CARTESIAN_POINT('',(3.5,4.,9.4));
#9214=CARTESIAN_POINT('Origin',(4.,4.,9.4));
#9215=CARTESIAN_POINT('',(3.5,4.,9.6));
#9216=CARTESIAN_POINT('',(3.5,4.,9.4));
#9217=CARTESIAN_POINT('Origin',(4.,4.,9.6));
#9218=CARTESIAN_POINT('Origin',(4.,4.,9.6));
#9219=CARTESIAN_POINT('',(3.59,4.,9.6));
#9220=CARTESIAN_POINT('Origin',(4.,4.,9.6));
#9221=CARTESIAN_POINT('Origin',(4.,4.,9.4));
#9222=CARTESIAN_POINT('',(3.59,4.,9.4));
#9223=CARTESIAN_POINT('Origin',(4.,4.,9.4));
#9224=CARTESIAN_POINT('Origin',(4.,4.,8.4));
#9225=CARTESIAN_POINT('',(3.59,4.,8.5));
#9226=CARTESIAN_POINT('Origin',(4.,4.,8.5));
#9227=CARTESIAN_POINT('',(3.59,4.,8.4));
#9228=CARTESIAN_POINT('Origin',(4.,4.,8.4));
#9229=CARTESIAN_POINT('',(3.59,4.,10.));
#9230=CARTESIAN_POINT('',(3.59,4.,8.4));
#9231=CARTESIAN_POINT('Origin',(4.,4.,10.));
#9232=CARTESIAN_POINT('Origin',(4.,4.,8.));
#9233=CARTESIAN_POINT('',(2.75,4.,8.));
#9234=CARTESIAN_POINT('Origin',(4.,4.,8.));
#9235=CARTESIAN_POINT('',(2.75,4.,8.1));
#9236=CARTESIAN_POINT('',(2.75,4.,8.));
#9237=CARTESIAN_POINT('Origin',(4.,4.,8.1));
#9238=CARTESIAN_POINT('Origin',(4.,4.,8.1));
#9239=CARTESIAN_POINT('',(3.,4.,8.1));
#9240=CARTESIAN_POINT('Origin',(4.,4.,8.1));
#9241=CARTESIAN_POINT('Origin',(4.,4.,7.9));
#9242=CARTESIAN_POINT('',(3.,4.,8.5));
#9243=CARTESIAN_POINT('',(3.,4.,7.9));
#9244=CARTESIAN_POINT('Origin',(4.,4.,8.5));
#9245=CARTESIAN_POINT('Origin',(4.,4.,8.5));
#9246=CARTESIAN_POINT('Origin',(2.72720779386421,2.72720779386421,7.9));
#9247=CARTESIAN_POINT('',(2.45220779386421,2.72720779386421,8.));
#9248=CARTESIAN_POINT('Origin',(2.72720779386421,2.72720779386421,8.));
#9249=CARTESIAN_POINT('',(2.45220779386421,2.72720779386421,10.));
#9250=CARTESIAN_POINT('',(2.45220779386421,2.72720779386421,7.9));
#9251=CARTESIAN_POINT('Origin',(2.72720779386421,2.72720779386421,10.));
#9252=CARTESIAN_POINT('Origin',(2.72720779386421,5.27279220613579,7.9));
#9253=CARTESIAN_POINT('',(2.45220779386421,5.27279220613579,8.));
#9254=CARTESIAN_POINT('Origin',(2.72720779386421,5.27279220613579,8.));
#9255=CARTESIAN_POINT('',(2.45220779386421,5.27279220613579,10.));
#9256=CARTESIAN_POINT('',(2.45220779386421,5.27279220613579,7.9));
#9257=CARTESIAN_POINT('Origin',(2.72720779386421,5.27279220613579,10.));
#9258=CARTESIAN_POINT('Origin',(5.27279220613579,5.27279220613579,7.9));
#9259=CARTESIAN_POINT('',(4.99779220613579,5.27279220613579,8.));
#9260=CARTESIAN_POINT('Origin',(5.27279220613579,5.27279220613579,8.));
#9261=CARTESIAN_POINT('',(4.99779220613579,5.27279220613579,10.));
#9262=CARTESIAN_POINT('',(4.99779220613579,5.27279220613579,7.9));
#9263=CARTESIAN_POINT('Origin',(5.27279220613579,5.27279220613579,10.));
#9264=CARTESIAN_POINT('Origin',(5.27279220613578,2.72720779386421,7.9));
#9265=CARTESIAN_POINT('',(4.99779220613578,2.72720779386421,8.));
#9266=CARTESIAN_POINT('Origin',(5.27279220613578,2.72720779386421,8.));
#9267=CARTESIAN_POINT('',(4.99779220613578,2.72720779386421,10.));
#9268=CARTESIAN_POINT('',(4.99779220613578,2.72720779386421,7.9));
#9269=CARTESIAN_POINT('Origin',(5.27279220613578,2.72720779386421,10.));
#9270=CARTESIAN_POINT('Origin',(4.,4.,8.));
#9271=CARTESIAN_POINT('',(1.6,4.,10.));
#9272=CARTESIAN_POINT('Origin',(4.,4.,10.));
#9273=CARTESIAN_POINT('',(1.6,4.,8.));
#9274=CARTESIAN_POINT('',(1.6,4.,8.));
#9275=CARTESIAN_POINT('Origin',(4.,4.,8.));
#9276=CARTESIAN_POINT('Origin',(4.,4.,10.));
#9277=CARTESIAN_POINT('Origin',(4.,4.,8.));
#9278=CARTESIAN_POINT('',(0.,0.,0.));
#9279=CARTESIAN_POINT('Origin',(4.,4.,8.));
#9280=CARTESIAN_POINT('',(3.,4.,8.1));
#9281=CARTESIAN_POINT('Origin',(4.,4.,8.1));
#9282=CARTESIAN_POINT('',(3.,4.,8.));
#9283=CARTESIAN_POINT('',(3.,4.,8.));
#9284=CARTESIAN_POINT('Origin',(4.,4.,8.));
#9285=CARTESIAN_POINT('Origin',(4.,4.,8.));
#9286=CARTESIAN_POINT('',(2.75,4.,8.1));
#9287=CARTESIAN_POINT('Origin',(4.,4.,8.1));
#9288=CARTESIAN_POINT('',(2.75,4.,8.));
#9289=CARTESIAN_POINT('',(2.75,4.,8.));
#9290=CARTESIAN_POINT('Origin',(4.,4.,8.));
#9291=CARTESIAN_POINT('Origin',(4.,4.,8.1));
#9292=CARTESIAN_POINT('Origin',(4.,4.,8.));
#9293=CARTESIAN_POINT('',(0.,0.,0.));
#9294=CARTESIAN_POINT('Origin',(4.,4.,2.));
#9295=CARTESIAN_POINT('',(3.,4.,8.));
#9296=CARTESIAN_POINT('Origin',(4.,4.,8.));
#9297=CARTESIAN_POINT('',(3.,4.,2.));
#9298=CARTESIAN_POINT('',(3.,4.,2.));
#9299=CARTESIAN_POINT('Origin',(4.,4.,2.));
#9300=CARTESIAN_POINT('Origin',(4.,4.,2.));
#9301=CARTESIAN_POINT('',(2.75,4.,8.));
#9302=CARTESIAN_POINT('Origin',(4.,4.,8.));
#9303=CARTESIAN_POINT('',(2.75,4.,2.));
#9304=CARTESIAN_POINT('',(2.75,4.,2.));
#9305=CARTESIAN_POINT('Origin',(4.,4.,2.));
#9306=CARTESIAN_POINT('Origin',(4.,4.,8.));
#9307=CARTESIAN_POINT('Origin',(4.,4.,2.));
#9308=CARTESIAN_POINT('',(0.,0.,0.));
#9309=CARTESIAN_POINT('Origin',(4.,4.,9.4));
#9310=CARTESIAN_POINT('',(3.6,4.,9.6));
#9311=CARTESIAN_POINT('Origin',(4.,4.,9.6));
#9312=CARTESIAN_POINT('',(3.6,4.,9.4));
#9313=CARTESIAN_POINT('',(3.6,4.,9.4));
#9314=CARTESIAN_POINT('Origin',(4.,4.,9.4));
#9315=CARTESIAN_POINT('Origin',(4.,4.,9.4));
#9316=CARTESIAN_POINT('',(3.5,4.,9.6));
#9317=CARTESIAN_POINT('Origin',(4.,4.,9.6));
#9318=CARTESIAN_POINT('',(3.5,4.,9.4));
#9319=CARTESIAN_POINT('',(3.5,4.,9.4));
#9320=CARTESIAN_POINT('Origin',(4.,4.,9.4));
#9321=CARTESIAN_POINT('Origin',(4.,4.,9.6));
#9322=CARTESIAN_POINT('Origin',(4.,4.,9.4));
#9323=CARTESIAN_POINT('',(0.,0.,0.));
#9324=CARTESIAN_POINT('Origin',(5.27279220613579,5.27279220613579,-1.8));
#9325=CARTESIAN_POINT('',(5.02279220613579,5.27279220613579,10.8));
#9326=CARTESIAN_POINT('Origin',(5.27279220613579,5.27279220613579,10.8));
#9327=CARTESIAN_POINT('',(5.02279220613579,5.27279220613579,-1.8));
#9328=CARTESIAN_POINT('',(5.02279220613579,5.27279220613579,-1.8));
#9329=CARTESIAN_POINT('Origin',(5.27279220613579,5.27279220613579,-1.8));
#9330=CARTESIAN_POINT('Origin',(5.27279220613579,5.27279220613579,10.8));
#9331=CARTESIAN_POINT('Origin',(5.27279220613579,5.27279220613579,-1.8));
#9332=CARTESIAN_POINT('',(0.,0.,0.));
#9333=CARTESIAN_POINT('Origin',(2.72720779386421,5.27279220613579,-1.8));
#9334=CARTESIAN_POINT('',(2.47720779386421,5.27279220613579,10.8));
#9335=CARTESIAN_POINT('Origin',(2.72720779386421,5.27279220613579,10.8));
#9336=CARTESIAN_POINT('',(2.47720779386421,5.27279220613579,-1.8));
#9337=CARTESIAN_POINT('',(2.47720779386421,5.27279220613579,-1.8));
#9338=CARTESIAN_POINT('Origin',(2.72720779386421,5.27279220613579,-1.8));
#9339=CARTESIAN_POINT('Origin',(2.72720779386421,5.27279220613579,10.8));
#9340=CARTESIAN_POINT('Origin',(2.72720779386421,5.27279220613579,-1.8));
#9341=CARTESIAN_POINT('',(0.,0.,0.));
#9342=CARTESIAN_POINT('Origin',(2.72720779386421,2.72720779386421,-1.8));
#9343=CARTESIAN_POINT('',(2.47720779386421,2.72720779386421,10.8));
#9344=CARTESIAN_POINT('Origin',(2.72720779386421,2.72720779386421,10.8));
#9345=CARTESIAN_POINT('',(2.47720779386421,2.72720779386421,-1.8));
#9346=CARTESIAN_POINT('',(2.47720779386421,2.72720779386421,-1.8));
#9347=CARTESIAN_POINT('Origin',(2.72720779386421,2.72720779386421,-1.8));
#9348=CARTESIAN_POINT('Origin',(2.72720779386421,2.72720779386421,10.8));
#9349=CARTESIAN_POINT('Origin',(2.72720779386421,2.72720779386421,-1.8));
#9350=CARTESIAN_POINT('',(0.,0.,0.));
#9351=CARTESIAN_POINT('Origin',(5.27279220613578,2.72720779386421,-1.8));
#9352=CARTESIAN_POINT('',(5.02279220613578,2.72720779386421,10.8));
#9353=CARTESIAN_POINT('Origin',(5.27279220613578,2.72720779386421,10.8));
#9354=CARTESIAN_POINT('',(5.02279220613578,2.72720779386421,-1.8));
#9355=CARTESIAN_POINT('',(5.02279220613578,2.72720779386421,-1.8));
#9356=CARTESIAN_POINT('Origin',(5.27279220613578,2.72720779386421,-1.8));
#9357=CARTESIAN_POINT('Origin',(5.27279220613578,2.72720779386421,10.8));
#9358=CARTESIAN_POINT('Origin',(5.27279220613578,2.72720779386421,-1.8));
#9359=CARTESIAN_POINT('',(0.,0.,0.));
#9360=CARTESIAN_POINT('',(0.,0.,0.));
#9361=CARTESIAN_POINT('Origin',(0.75,1.2,0.));
#9362=CARTESIAN_POINT('',(0.885663593019381,1.2,-0.16));
#9363=CARTESIAN_POINT('',(0.885663593019381,1.2,0.16));
#9364=CARTESIAN_POINT('Origin',(0.,1.2,0.));
#9365=CARTESIAN_POINT('',(0.93,1.2,-0.16));
#9366=CARTESIAN_POINT('',(0.93,1.2,-0.16));
#9367=CARTESIAN_POINT('',(0.93,1.2,0.16));
#9368=CARTESIAN_POINT('',(0.93,1.2,0.16));
#9369=CARTESIAN_POINT('',(0.57,1.2,0.16));
#9370=CARTESIAN_POINT('Origin',(0.57,0.,0.16));
#9371=CARTESIAN_POINT('',(0.885663593019381,-1.2,0.16));
#9372=CARTESIAN_POINT('',(0.885663593019381,0.,0.16));
#9373=CARTESIAN_POINT('',(0.93,-1.2,0.16));
#9374=CARTESIAN_POINT('',(0.93,0.,0.16));
#9375=CARTESIAN_POINT('',(0.57,-1.2,0.16));
#9376=CARTESIAN_POINT('Origin',(0.75,-1.2,0.));
#9377=CARTESIAN_POINT('',(0.885663593019381,-1.2,-0.16));
#9378=CARTESIAN_POINT('Origin',(0.,-1.2,0.));
#9379=CARTESIAN_POINT('',(0.93,-1.2,-0.16));
#9380=CARTESIAN_POINT('',(0.93,-1.2,0.16));
#9381=CARTESIAN_POINT('',(0.93,-1.2,-0.16));
#9382=CARTESIAN_POINT('Origin',(0.93,0.,-0.16));
#9383=CARTESIAN_POINT('',(0.885663593019381,0.,-0.16));
#9384=CARTESIAN_POINT('',(0.93,0.,-0.16));
#9385=CARTESIAN_POINT('Origin',(0.93,0.,0.16));
#9386=CARTESIAN_POINT('Origin',(1.05,1.5,0.));
#9387=CARTESIAN_POINT('',(-1.05,1.5,-1.28587913910472E-16));
#9388=CARTESIAN_POINT('Origin',(0.,1.5,0.));
#9389=CARTESIAN_POINT('',(-0.9,1.5,-1.10218211923262E-16));
#9390=CARTESIAN_POINT('Origin',(0.,1.5,0.));
#9391=CARTESIAN_POINT('Origin',(0.,1.315,0.));
#9392=CARTESIAN_POINT('',(-1.05,1.13,-1.28587913910472E-16));
#9393=CARTESIAN_POINT('Origin',(0.,1.13,0.));
#9394=CARTESIAN_POINT('',(-1.05,1.315,-1.28587913910472E-16));
#9395=CARTESIAN_POINT('Origin',(1.,1.13,0.));
#9396=CARTESIAN_POINT('',(-1.,1.13,-1.22464679914735E-16));
#9397=CARTESIAN_POINT('Origin',(0.,1.13,0.));
#9398=CARTESIAN_POINT('Origin',(0.,1.065,0.));
#9399=CARTESIAN_POINT('',(-1.,1.,-1.22464679914735E-16));
#9400=CARTESIAN_POINT('Origin',(0.,1.,0.));
#9401=CARTESIAN_POINT('',(-1.,1.065,-1.22464679914735E-16));
#9402=CARTESIAN_POINT('Origin',(1.05,1.,0.));
#9403=CARTESIAN_POINT('',(-1.05,1.,-1.28587913910472E-16));
#9404=CARTESIAN_POINT('Origin',(0.,1.,0.));
#9405=CARTESIAN_POINT('Origin',(0.,0.,0.));
#9406=CARTESIAN_POINT('',(-1.05,-1.,-1.28587913910472E-16));
#9407=CARTESIAN_POINT('Origin',(0.,-1.,0.));
#9408=CARTESIAN_POINT('',(-1.05,0.,-1.28587913910472E-16));
#9409=CARTESIAN_POINT('Origin',(1.,-1.,0.));
#9410=CARTESIAN_POINT('',(-1.,-1.,-1.22464679914735E-16));
#9411=CARTESIAN_POINT('Origin',(0.,-1.,0.));
#9412=CARTESIAN_POINT('Origin',(0.,-1.065,0.));
#9413=CARTESIAN_POINT('',(-1.,-1.13,-1.22464679914735E-16));
#9414=CARTESIAN_POINT('Origin',(0.,-1.13,0.));
#9415=CARTESIAN_POINT('',(-1.,-1.065,-1.22464679914735E-16));
#9416=CARTESIAN_POINT('Origin',(1.05,-1.13,0.));
#9417=CARTESIAN_POINT('',(-1.05,-1.13,-1.28587913910472E-16));
#9418=CARTESIAN_POINT('Origin',(0.,-1.13,0.));
#9419=CARTESIAN_POINT('Origin',(0.,-1.315,0.));
#9420=CARTESIAN_POINT('',(-1.05,-1.5,-1.28587913910472E-16));
#9421=CARTESIAN_POINT('Origin',(0.,-1.5,0.));
#9422=CARTESIAN_POINT('',(-1.05,-1.315,-1.28587913910472E-16));
#9423=CARTESIAN_POINT('Origin',(0.9,-1.5,0.));
#9424=CARTESIAN_POINT('',(-0.9,-1.5,-1.10218211923262E-16));
#9425=CARTESIAN_POINT('Origin',(0.,-1.5,0.));
#9426=CARTESIAN_POINT('Origin',(0.,0.,0.));
#9427=CARTESIAN_POINT('',(-0.9,0.,-1.10218211923262E-16));
#9428=CARTESIAN_POINT('',(0.,0.,0.));
#9429=CARTESIAN_POINT('Origin',(0.75,1.2,0.));
#9430=CARTESIAN_POINT('',(0.880582193778639,1.2,0.16));
#9431=CARTESIAN_POINT('',(0.880582193778639,1.2,-0.16));
#9432=CARTESIAN_POINT('Origin',(0.,1.2,0.));
#9433=CARTESIAN_POINT('',(0.583459510163302,1.2,0.16));
#9434=CARTESIAN_POINT('',(0.57,1.2,0.16));
#9435=CARTESIAN_POINT('',(0.583459510163302,1.2,-0.16));
#9436=CARTESIAN_POINT('Origin',(0.,1.2,0.));
#9437=CARTESIAN_POINT('',(0.93,1.2,-0.16));
#9438=CARTESIAN_POINT('Origin',(0.93,0.,-0.16));
#9439=CARTESIAN_POINT('',(0.880582193778639,-1.2,-0.16));
#9440=CARTESIAN_POINT('',(0.880582193778639,0.,-0.16));
#9441=CARTESIAN_POINT('',(0.583459510163302,-1.2,-0.16));
#9442=CARTESIAN_POINT('',(0.583459510163302,0.,-0.16));
#9443=CARTESIAN_POINT('',(0.93,-1.2,-0.16));
#9444=CARTESIAN_POINT('Origin',(0.75,-1.2,0.));
#9445=CARTESIAN_POINT('',(0.880582193778639,-1.2,0.16));
#9446=CARTESIAN_POINT('Origin',(0.,-1.2,0.));
#9447=CARTESIAN_POINT('',(0.583459510163302,-1.2,0.16));
#9448=CARTESIAN_POINT('Origin',(0.,-1.2,0.));
#9449=CARTESIAN_POINT('',(0.57,-1.2,0.16));
#9450=CARTESIAN_POINT('Origin',(0.57,0.,0.16));
#9451=CARTESIAN_POINT('',(0.880582193778639,0.,0.16));
#9452=CARTESIAN_POINT('',(0.583459510163302,0.,0.16));
#9453=CARTESIAN_POINT('Origin',(0.895,1.35,0.));
#9454=CARTESIAN_POINT('',(-0.895,1.35,-1.09605888523688E-16));
#9455=CARTESIAN_POINT('Origin',(0.,1.35,0.));
#9456=CARTESIAN_POINT('',(-0.605,1.35,-7.40911313484149E-17));
#9457=CARTESIAN_POINT('Origin',(0.,1.35,0.));
#9458=CARTESIAN_POINT('Origin',(0.,0.,0.));
#9459=CARTESIAN_POINT('',(-0.895,-1.35,-1.09605888523688E-16));
#9460=CARTESIAN_POINT('Origin',(0.,-1.35,0.));
#9461=CARTESIAN_POINT('',(-0.895,0.,-1.09605888523688E-16));
#9462=CARTESIAN_POINT('Origin',(0.605,-1.35,0.));
#9463=CARTESIAN_POINT('',(-0.605,-1.35,-7.40911313484149E-17));
#9464=CARTESIAN_POINT('Origin',(0.,-1.35,0.));
#9465=CARTESIAN_POINT('Origin',(0.,0.,0.));
#9466=CARTESIAN_POINT('',(-0.605,0.,-7.40911313484149E-17));
#9467=CARTESIAN_POINT('',(0.,0.,0.));
#9468=CARTESIAN_POINT('',(0.,0.,0.));
#9469=CARTESIAN_POINT('',(0.,0.,0.));
#9470=CARTESIAN_POINT('Origin',(0.375,0.5,0.));
#9471=CARTESIAN_POINT('',(-0.375,0.5,-4.59242549680257E-17));
#9472=CARTESIAN_POINT('Origin',(0.,0.5,0.));
#9473=CARTESIAN_POINT('Origin',(0.,0.475,0.));
#9474=CARTESIAN_POINT('',(-0.425,0.45,-5.20474889637625E-17));
#9475=CARTESIAN_POINT('Origin',(0.,0.45,0.));
#9476=CARTESIAN_POINT('',(-0.4,0.475,-4.89858719658941E-17));
#9477=CARTESIAN_POINT('Origin',(0.,0.24,0.));
#9478=CARTESIAN_POINT('',(-0.425,0.0299999999999998,-5.20474889637625E-17));
#9479=CARTESIAN_POINT('Origin',(0.,0.0299999999999998,0.));
#9480=CARTESIAN_POINT('',(-0.425,0.24,-5.20474889637625E-17));
#9481=CARTESIAN_POINT('Origin',(0.,0.0150000000000001,0.));
#9482=CARTESIAN_POINT('',(-0.395,4.85722573273506E-17,-4.83735485663204E-17));
#9483=CARTESIAN_POINT('Origin',(0.,0.,0.));
#9484=CARTESIAN_POINT('',(-0.41,0.0150000000000001,-5.02105187650415E-17));
#9485=CARTESIAN_POINT('Origin',(0.27,0.,0.));
#9486=CARTESIAN_POINT('',(-0.27,0.,-3.30654635769785E-17));
#9487=CARTESIAN_POINT('Origin',(0.,0.,0.));
#9488=CARTESIAN_POINT('Origin',(0.,-0.02,0.));
#9489=CARTESIAN_POINT('',(-0.24505,-0.0498999999999999,3.00099698131059E-17));
#9490=CARTESIAN_POINT('Origin',(0.,-0.0498999999999999,0.));
#9491=CARTESIAN_POINT('',(-0.26,-0.02,-3.18408167778312E-17));
#9492=CARTESIAN_POINT('Origin',(0.,-0.995,0.));
#9493=CARTESIAN_POINT('',(-0.24505,-1.95495,3.00099698131059E-17));
#9494=CARTESIAN_POINT('Origin',(0.,-1.95495,0.));
#9495=CARTESIAN_POINT('',(-0.24505,-0.995,-3.00099698131059E-17));
#9496=CARTESIAN_POINT('Origin',(0.,-1.975,0.));
#9497=CARTESIAN_POINT('',(-0.2,-2.,-2.44929359829471E-17));
#9498=CARTESIAN_POINT('Origin',(0.,-2.,0.));
#9499=CARTESIAN_POINT('',(-0.225,-1.975,-2.75545529808154E-17));
#9500=CARTESIAN_POINT('Origin',(0.,-2.,0.));
#9501=CARTESIAN_POINT('Origin',(0.115470053837925,-0.5,-0.2));
#9502=CARTESIAN_POINT('',(0.23094010767585,-0.5,0.));
#9503=CARTESIAN_POINT('',(0.115470053837925,-0.5,-0.2));
#9504=CARTESIAN_POINT('',(0.23094010767585,-0.5,0.));
#9505=CARTESIAN_POINT('',(0.115470053837925,-0.8,-0.2));
#9506=CARTESIAN_POINT('',(0.115470053837925,-0.5,-0.2));
#9507=CARTESIAN_POINT('',(0.23094010767585,-0.8,0.));
#9508=CARTESIAN_POINT('',(0.23094010767585,-0.8,0.));
#9509=CARTESIAN_POINT('',(0.23094010767585,-0.5,0.));
#9510=CARTESIAN_POINT('Origin',(-0.115470053837925,-0.5,-0.2));
#9511=CARTESIAN_POINT('',(-0.115470053837925,-0.5,-0.2));
#9512=CARTESIAN_POINT('',(0.115470053837925,-0.5,-0.2));
#9513=CARTESIAN_POINT('',(-0.115470053837925,-0.8,-0.2));
#9514=CARTESIAN_POINT('',(-0.115470053837925,-0.5,-0.2));
#9515=CARTESIAN_POINT('',(0.115470053837925,-0.8,-0.2));
#9516=CARTESIAN_POINT('Origin',(-0.23094010767585,-0.5,-2.77555756156289E-17));
#9517=CARTESIAN_POINT('',(-0.23094010767585,-0.5,-2.82820063659975E-17));
#9518=CARTESIAN_POINT('',(-0.115470053837925,-0.5,-0.2));
#9519=CARTESIAN_POINT('',(-0.23094010767585,-0.8,-2.77555756156289E-17));
#9520=CARTESIAN_POINT('',(-0.23094010767585,-0.5,-2.82820063659975E-17));
#9521=CARTESIAN_POINT('',(-0.115470053837925,-0.8,-0.2));
#9522=CARTESIAN_POINT('Origin',(-0.115470053837925,-0.5,0.2));
#9523=CARTESIAN_POINT('',(-0.115470053837925,-0.5,0.2));
#9524=CARTESIAN_POINT('',(-0.23094010767585,-0.5,-2.82820063659975E-17));
#9525=CARTESIAN_POINT('',(-0.115470053837925,-0.8,0.2));
#9526=CARTESIAN_POINT('',(-0.115470053837925,-0.5,0.2));
#9527=CARTESIAN_POINT('',(-0.23094010767585,-0.8,-2.82820063659975E-17));
#9528=CARTESIAN_POINT('Origin',(0.115470053837925,-0.5,0.2));
#9529=CARTESIAN_POINT('',(0.115470053837925,-0.5,0.2));
#9530=CARTESIAN_POINT('',(-0.115470053837925,-0.5,0.2));
#9531=CARTESIAN_POINT('',(0.115470053837925,-0.8,0.2));
#9532=CARTESIAN_POINT('',(0.115470053837925,-0.5,0.2));
#9533=CARTESIAN_POINT('',(-0.115470053837925,-0.8,0.2));
#9534=CARTESIAN_POINT('Origin',(0.23094010767585,-0.5,0.));
#9535=CARTESIAN_POINT('',(0.115470053837925,-0.5,0.2));
#9536=CARTESIAN_POINT('',(0.115470053837925,-0.8,0.2));
#9537=CARTESIAN_POINT('Origin',(0.,-0.5,0.));
#9538=CARTESIAN_POINT('Origin',(0.,-0.8,0.));
#9539=CARTESIAN_POINT('',(0.,0.,0.));
#9540=CARTESIAN_POINT('',(0.,0.,0.));
#9541=CARTESIAN_POINT('Origin',(0.,0.6,0.));
#9542=CARTESIAN_POINT('',(-0.43,0.6,5.26598123633362E-17));
#9543=CARTESIAN_POINT('Origin',(0.,0.6,0.));
#9544=CARTESIAN_POINT('',(-0.43,0.7,-5.26598123633362E-17));
#9545=CARTESIAN_POINT('',(-0.43,0.6,5.26598123633362E-17));
#9546=CARTESIAN_POINT('Origin',(0.,0.7,0.));
#9547=CARTESIAN_POINT('Origin',(0.,0.6,0.));
#9548=CARTESIAN_POINT('',(-0.2,0.6,2.44929359829471E-17));
#9549=CARTESIAN_POINT('Origin',(0.,0.6,0.));
#9550=CARTESIAN_POINT('Origin',(0.,0.5,-1.11022302462516E-16));
#9551=CARTESIAN_POINT('',(0.346410161513776,0.5,0.6));
#9552=CARTESIAN_POINT('',(0.692820323027551,0.5,0.));
#9553=CARTESIAN_POINT('',(0.346410161513776,0.5,0.6));
#9554=CARTESIAN_POINT('',(0.346410161513776,0.5,-0.6));
#9555=CARTESIAN_POINT('',(0.692820323027551,0.5,0.));
#9556=CARTESIAN_POINT('',(-0.346410161513775,0.5,-0.6));
#9557=CARTESIAN_POINT('',(0.346410161513776,0.5,-0.6));
#9558=CARTESIAN_POINT('',(-0.692820323027551,0.5,-8.48460190979926E-17));
#9559=CARTESIAN_POINT('',(-0.346410161513775,0.5,-0.6));
#9560=CARTESIAN_POINT('',(-0.346410161513776,0.5,0.6));
#9561=CARTESIAN_POINT('',(-0.692820323027551,0.5,-8.48460190979926E-17));
#9562=CARTESIAN_POINT('',(-0.346410161513776,0.5,0.6));
#9563=CARTESIAN_POINT('',(-0.525,0.5,-6.4293956955236E-17));
#9564=CARTESIAN_POINT('Origin',(0.,0.5,0.));
#9565=CARTESIAN_POINT('Origin',(0.,0.,-1.11022302462516E-16));
#9566=CARTESIAN_POINT('',(0.346410161513776,0.,0.6));
#9567=CARTESIAN_POINT('',(0.692820323027551,0.,0.));
#9568=CARTESIAN_POINT('',(0.346410161513776,0.,0.6));
#9569=CARTESIAN_POINT('',(-0.346410161513776,0.,0.6));
#9570=CARTESIAN_POINT('',(-0.346410161513776,0.,0.6));
#9571=CARTESIAN_POINT('',(-0.692820323027551,0.,-8.48460190979926E-17));
#9572=CARTESIAN_POINT('',(-0.692820323027551,0.,-8.48460190979926E-17));
#9573=CARTESIAN_POINT('',(-0.346410161513775,0.,-0.6));
#9574=CARTESIAN_POINT('',(-0.346410161513775,0.,-0.6));
#9575=CARTESIAN_POINT('',(0.346410161513776,0.,-0.6));
#9576=CARTESIAN_POINT('',(0.346410161513776,0.,-0.6));
#9577=CARTESIAN_POINT('',(0.692820323027551,0.,0.));
#9578=CARTESIAN_POINT('',(-0.515,0.,-6.30693101560887E-17));
#9579=CARTESIAN_POINT('Origin',(0.,0.,0.));
#9580=CARTESIAN_POINT('Origin',(-0.346410161513776,0.,0.6));
#9581=CARTESIAN_POINT('',(0.346410161513776,0.,0.6));
#9582=CARTESIAN_POINT('',(-0.346410161513776,0.,0.6));
#9583=CARTESIAN_POINT('Origin',(-0.692820323027551,0.,-8.48460190979926E-17));
#9584=CARTESIAN_POINT('',(-0.692820323027551,0.,-8.48460190979926E-17));
#9585=CARTESIAN_POINT('Origin',(-0.346410161513775,0.,-0.6));
#9586=CARTESIAN_POINT('',(-0.346410161513775,0.,-0.6));
#9587=CARTESIAN_POINT('Origin',(0.346410161513776,0.,-0.6));
#9588=CARTESIAN_POINT('',(0.346410161513776,0.,-0.6));
#9589=CARTESIAN_POINT('Origin',(0.692820323027551,0.,0.));
#9590=CARTESIAN_POINT('',(0.692820323027551,0.,0.));
#9591=CARTESIAN_POINT('Origin',(0.346410161513776,0.,0.6));
#9592=CARTESIAN_POINT('Origin',(0.46,0.7,0.));
#9593=CARTESIAN_POINT('',(-0.46,0.7,-5.63337527607782E-17));
#9594=CARTESIAN_POINT('Origin',(0.,0.7,0.));
#9595=CARTESIAN_POINT('Origin',(0.,1.2,0.));
#9596=CARTESIAN_POINT('',(-0.46,1.7,-5.63337527607782E-17));
#9597=CARTESIAN_POINT('',(-0.46,1.2,-5.63337527607782E-17));
#9598=CARTESIAN_POINT('Origin',(0.,1.7,0.));
#9599=CARTESIAN_POINT('Origin',(0.525,1.7,0.));
#9600=CARTESIAN_POINT('',(-0.525,1.7,-6.4293956955236E-17));
#9601=CARTESIAN_POINT('Origin',(0.,1.7,0.));
#9602=CARTESIAN_POINT('Origin',(0.,1.1,0.));
#9603=CARTESIAN_POINT('',(-0.525,1.1,-6.4293956955236E-17));
#9604=CARTESIAN_POINT('Origin',(0.,-0.325,0.));
#9605=CARTESIAN_POINT('',(-0.515,-0.65,-6.30693101560887E-17));
#9606=CARTESIAN_POINT('Origin',(0.,-0.65,0.));
#9607=CARTESIAN_POINT('',(-0.515,-0.325,-6.30693101560887E-17));
#9608=CARTESIAN_POINT('Origin',(0.2,-0.65,0.));
#9609=CARTESIAN_POINT('',(-0.2,-0.65,-2.44929359829471E-17));
#9610=CARTESIAN_POINT('Origin',(0.,-0.65,0.));
#9611=CARTESIAN_POINT('Origin',(0.,0.0249999999999999,0.));
#9612=CARTESIAN_POINT('',(-0.2,0.0249999999999999,-2.44929359829471E-17));
#9613=CARTESIAN_POINT('',(0.,0.,0.));
#9614=CARTESIAN_POINT('Origin',(0.475,1.95,0.));
#9615=CARTESIAN_POINT('',(-0.475,1.95,-5.81707229594993E-17));
#9616=CARTESIAN_POINT('Origin',(0.,1.95,0.));
#9617=CARTESIAN_POINT('',(-0.31,1.95,-3.7964050773568E-17));
#9618=CARTESIAN_POINT('Origin',(0.,1.95,0.));
#9619=CARTESIAN_POINT('Origin',(0.,1.825,0.));
#9620=CARTESIAN_POINT('',(-0.475,1.7,-5.81707229594993E-17));
#9621=CARTESIAN_POINT('Origin',(0.,1.7,0.));
#9622=CARTESIAN_POINT('',(-0.475,1.825,-5.81707229594993E-17));
#9623=CARTESIAN_POINT('Origin',(0.355,1.7,0.));
#9624=CARTESIAN_POINT('',(-0.355,1.7,-4.3474961369731E-17));
#9625=CARTESIAN_POINT('Origin',(0.,1.7,0.));
#9626=CARTESIAN_POINT('Origin',(0.,1.55,0.));
#9627=CARTESIAN_POINT('',(-0.355,1.4,-4.3474961369731E-17));
#9628=CARTESIAN_POINT('Origin',(0.,1.4,0.));
#9629=CARTESIAN_POINT('',(-0.355,1.55,-4.3474961369731E-17));
#9630=CARTESIAN_POINT('Origin',(0.31,1.4,0.));
#9631=CARTESIAN_POINT('',(-0.31,1.4,-3.7964050773568E-17));
#9632=CARTESIAN_POINT('Origin',(0.,1.4,0.));
#9633=CARTESIAN_POINT('Origin',(0.,1.675,0.));
#9634=CARTESIAN_POINT('',(-0.31,1.675,-3.7964050773568E-17));
#9635=CARTESIAN_POINT('',(0.,0.,0.));
#9636=CARTESIAN_POINT('',(0.,0.,0.));
#9637=CARTESIAN_POINT('',(0.,0.,0.));
#9638=CARTESIAN_POINT('Origin',(0.,0.09,0.));
#9639=CARTESIAN_POINT('',(-0.285,0.1,3.49024337756996E-17));
#9640=CARTESIAN_POINT('Origin',(0.,0.1,0.));
#9641=CARTESIAN_POINT('',(-0.265,0.08,-3.24531401774049E-17));
#9642=CARTESIAN_POINT('',(-0.275,0.09,3.36777869765522E-17));
#9643=CARTESIAN_POINT('Origin',(0.,0.08,0.));
#9644=CARTESIAN_POINT('Origin',(0.,0.,0.));
#9645=CARTESIAN_POINT('',(-0.265,0.,3.24531401774049E-17));
#9646=CARTESIAN_POINT('',(-0.265,0.,3.24531401774049E-17));
#9647=CARTESIAN_POINT('Origin',(0.,0.,0.));
#9648=CARTESIAN_POINT('Origin',(0.,0.1,0.));
#9649=CARTESIAN_POINT('',(-0.5,0.1,6.12323399573677E-17));
#9650=CARTESIAN_POINT('Origin',(0.,0.1,0.));
#9651=CARTESIAN_POINT('Origin',(0.,0.,0.));
#9652=CARTESIAN_POINT('',(-0.5,0.,6.12323399573677E-17));
#9653=CARTESIAN_POINT('',(-0.5,0.,6.12323399573677E-17));
#9654=CARTESIAN_POINT('Origin',(0.,0.,0.));
#9655=CARTESIAN_POINT('Origin',(0.,0.,0.));
#9656=CARTESIAN_POINT('',(0.,0.,0.));
#9657=CARTESIAN_POINT('Origin',(0.,0.0525042956467857,0.));
#9658=CARTESIAN_POINT('',(-0.230940107675851,0.0472735643746089,0.4));
#9659=CARTESIAN_POINT('',(0.23094010767585,0.0472735643746089,0.4));
#9660=CARTESIAN_POINT('Ctrl Pts',(-0.230940107675851,0.0472735643746089,
0.4));
#9661=CARTESIAN_POINT('Ctrl Pts',(1.11022302462516E-16,-0.0193931022920578,
0.4));
#9662=CARTESIAN_POINT('Ctrl Pts',(0.23094010767585,0.0472735643746089,0.4));
#9663=CARTESIAN_POINT('',(-0.461880215351701,0.0472735643746089,-5.6564012731995E-17));
#9664=CARTESIAN_POINT('Ctrl Pts',(-0.461880215351701,0.0472735643746089,
-5.6564012731995E-17));
#9665=CARTESIAN_POINT('Ctrl Pts',(-0.346410161513776,-0.0193931022920579,
0.2));
#9666=CARTESIAN_POINT('Ctrl Pts',(-0.230940107675851,0.0472735643746089,
0.4));
#9667=CARTESIAN_POINT('',(-0.38,-2.08166817117217E-17,-4.65365783675994E-17));
#9668=CARTESIAN_POINT('',(-0.47094010767585,0.0525042956467857,-5.7673529545534E-17));
#9669=CARTESIAN_POINT('Origin',(0.,0.,0.));
#9670=CARTESIAN_POINT('',(-0.23094010767585,0.0472735643746089,-0.4));
#9671=CARTESIAN_POINT('Ctrl Pts',(-0.23094010767585,0.0472735643746089,
-0.4));
#9672=CARTESIAN_POINT('Ctrl Pts',(-0.346410161513775,-0.0193931022920578,
-0.2));
#9673=CARTESIAN_POINT('Ctrl Pts',(-0.461880215351701,0.0472735643746089,
-5.6564012731995E-17));
#9674=CARTESIAN_POINT('',(0.23094010767585,0.0472735643746089,-0.4));
#9675=CARTESIAN_POINT('Ctrl Pts',(0.23094010767585,0.0472735643746089,-0.4));
#9676=CARTESIAN_POINT('Ctrl Pts',(0.,-0.0193931022920578,-0.4));
#9677=CARTESIAN_POINT('Ctrl Pts',(-0.23094010767585,0.0472735643746089,
-0.4));
#9678=CARTESIAN_POINT('',(0.461880215351701,0.0472735643746089,0.));
#9679=CARTESIAN_POINT('Ctrl Pts',(0.461880215351701,0.0472735643746089,
0.));
#9680=CARTESIAN_POINT('Ctrl Pts',(0.346410161513776,-0.019393102292058,
-0.2));
#9681=CARTESIAN_POINT('Ctrl Pts',(0.23094010767585,0.0472735643746089,-0.4));
#9682=CARTESIAN_POINT('Ctrl Pts',(0.23094010767585,0.0472735643746089,0.4));
#9683=CARTESIAN_POINT('Ctrl Pts',(0.346410161513776,-0.0193931022920577,
0.2));
#9684=CARTESIAN_POINT('Ctrl Pts',(0.461880215351701,0.0472735643746089,
0.));
#9685=CARTESIAN_POINT('Origin',(0.,0.417495704353214,0.));
#9686=CARTESIAN_POINT('',(-0.38,0.47,-4.65365783675994E-17));
#9687=CARTESIAN_POINT('Origin',(0.,0.47,0.));
#9688=CARTESIAN_POINT('',(-0.461880215351701,0.422726435625391,-5.6564012731995E-17));
#9689=CARTESIAN_POINT('',(-0.47094010767585,0.417495704353214,-5.7673529545534E-17));
#9690=CARTESIAN_POINT('',(-0.230940107675851,0.422726435625391,0.4));
#9691=CARTESIAN_POINT('Ctrl Pts',(-0.230940107675851,0.422726435625391,
0.4));
#9692=CARTESIAN_POINT('Ctrl Pts',(-0.346410161513776,0.489393102292058,
0.2));
#9693=CARTESIAN_POINT('Ctrl Pts',(-0.461880215351701,0.422726435625391,
-5.6564012731995E-17));
#9694=CARTESIAN_POINT('',(0.23094010767585,0.422726435625391,0.4));
#9695=CARTESIAN_POINT('Ctrl Pts',(0.23094010767585,0.422726435625391,0.4));
#9696=CARTESIAN_POINT('Ctrl Pts',(8.32667268468867E-17,0.489393102292058,
0.4));
#9697=CARTESIAN_POINT('Ctrl Pts',(-0.230940107675851,0.422726435625391,
0.4));
#9698=CARTESIAN_POINT('',(0.461880215351701,0.422726435625391,0.));
#9699=CARTESIAN_POINT('Ctrl Pts',(0.461880215351701,0.422726435625391,0.));
#9700=CARTESIAN_POINT('Ctrl Pts',(0.346410161513776,0.489393102292058,0.2));
#9701=CARTESIAN_POINT('Ctrl Pts',(0.23094010767585,0.422726435625391,0.4));
#9702=CARTESIAN_POINT('',(0.23094010767585,0.422726435625391,-0.4));
#9703=CARTESIAN_POINT('Ctrl Pts',(0.23094010767585,0.422726435625391,-0.4));
#9704=CARTESIAN_POINT('Ctrl Pts',(0.346410161513775,0.489393102292058,-0.2));
#9705=CARTESIAN_POINT('Ctrl Pts',(0.461880215351701,0.422726435625391,0.));
#9706=CARTESIAN_POINT('',(-0.23094010767585,0.422726435625391,-0.4));
#9707=CARTESIAN_POINT('Ctrl Pts',(-0.23094010767585,0.422726435625391,-0.4));
#9708=CARTESIAN_POINT('Ctrl Pts',(-5.55111512312578E-17,0.489393102292058,
-0.4));
#9709=CARTESIAN_POINT('Ctrl Pts',(0.23094010767585,0.422726435625391,-0.4));
#9710=CARTESIAN_POINT('Ctrl Pts',(-0.461880215351701,0.422726435625391,
-5.6564012731995E-17));
#9711=CARTESIAN_POINT('Ctrl Pts',(-0.346410161513776,0.489393102292058,
-0.2));
#9712=CARTESIAN_POINT('Ctrl Pts',(-0.23094010767585,0.422726435625391,-0.4));
#9713=CARTESIAN_POINT('Origin',(0.23094010767585,0.,-0.4));
#9714=CARTESIAN_POINT('',(-0.23094010767585,0.,-0.4));
#9715=CARTESIAN_POINT('',(0.23094010767585,0.,-0.4));
#9716=CARTESIAN_POINT('Origin',(-0.23094010767585,0.,-0.4));
#9717=CARTESIAN_POINT('',(-0.461880215351701,0.,-5.6564012731995E-17));
#9718=CARTESIAN_POINT('Origin',(-0.461880215351701,0.,-5.6564012731995E-17));
#9719=CARTESIAN_POINT('',(-0.230940107675851,0.,0.4));
#9720=CARTESIAN_POINT('Origin',(0.,0.,0.));
#9721=CARTESIAN_POINT('',(-0.2117,0.47,2.59257727379495E-17));
#9722=CARTESIAN_POINT('Origin',(0.,0.47,0.));
#9723=CARTESIAN_POINT('',(-0.2117,0.,2.59257727379495E-17));
#9724=CARTESIAN_POINT('',(-0.2117,0.,2.59257727379495E-17));
#9725=CARTESIAN_POINT('Origin',(0.,0.,0.));
#9726=CARTESIAN_POINT('Origin',(-0.230940107675851,0.,0.4));
#9727=CARTESIAN_POINT('',(0.23094010767585,0.,0.4));
#9728=CARTESIAN_POINT('Origin',(0.461880215351701,0.,0.));
#9729=CARTESIAN_POINT('',(0.461880215351701,0.,0.));
#9730=CARTESIAN_POINT('Origin',(0.23094010767585,0.,0.4));
#9731=CARTESIAN_POINT('Origin',(0.,0.47,0.));
#9732=CARTESIAN_POINT('Origin',(0.,0.,0.));
#9733=CARTESIAN_POINT('',(0.,0.,0.));
#9734=CARTESIAN_POINT('',(0.,0.,0.));
#9735=CARTESIAN_POINT('Origin',(4.,4.,13.4));
#9736=CARTESIAN_POINT('',(3.6,4.,13.4));
#9737=CARTESIAN_POINT('Origin',(4.,4.,13.4));
#9738=CARTESIAN_POINT('',(3.6,4.,13.8));
#9739=CARTESIAN_POINT('',(3.6,4.,13.4));
#9740=CARTESIAN_POINT('Origin',(4.,4.,13.8));
#9741=CARTESIAN_POINT('Origin',(4.,4.,13.4));
#9742=CARTESIAN_POINT('',(3.775,4.,13.4));
#9743=CARTESIAN_POINT('Origin',(4.,4.,13.4));
#9744=CARTESIAN_POINT('Origin',(4.,4.,12.9));
#9745=CARTESIAN_POINT('',(3.775,4.,13.));
#9746=CARTESIAN_POINT('Origin',(4.,4.,13.));
#9747=CARTESIAN_POINT('',(3.775,4.,12.9));
#9748=CARTESIAN_POINT('Origin',(2.,5.,13.));
#9749=CARTESIAN_POINT('',(2.,0.4,13.8));
#9750=CARTESIAN_POINT('',(2.,0.4,13.));
#9751=CARTESIAN_POINT('',(2.,0.4,13.));
#9752=CARTESIAN_POINT('',(2.,5.,13.8));
#9753=CARTESIAN_POINT('',(2.,5.,13.8));
#9754=CARTESIAN_POINT('',(2.,5.,13.));
#9755=CARTESIAN_POINT('',(2.,5.,13.));
#9756=CARTESIAN_POINT('',(2.,5.,13.));
#9757=CARTESIAN_POINT('Origin',(5.,5.,13.));
#9758=CARTESIAN_POINT('',(5.,5.,13.));
#9759=CARTESIAN_POINT('',(5.,5.,13.));
#9760=CARTESIAN_POINT('',(5.,5.,13.8));
#9761=CARTESIAN_POINT('',(5.,5.,13.8));
#9762=CARTESIAN_POINT('',(5.,5.,13.));
#9763=CARTESIAN_POINT('Origin',(5.,0.,13.));
#9764=CARTESIAN_POINT('',(5.,0.,13.));
#9765=CARTESIAN_POINT('',(5.,0.,13.));
#9766=CARTESIAN_POINT('',(5.,0.,13.8));
#9767=CARTESIAN_POINT('',(5.,0.,13.8));
#9768=CARTESIAN_POINT('',(5.,0.,13.));
#9769=CARTESIAN_POINT('Origin',(2.,0.,13.));
#9770=CARTESIAN_POINT('',(4.,0.,13.));
#9771=CARTESIAN_POINT('',(4.,0.,13.8));
#9772=CARTESIAN_POINT('',(4.,0.,13.));
#9773=CARTESIAN_POINT('',(2.,0.,13.));
#9774=CARTESIAN_POINT('',(2.,0.,13.8));
#9775=CARTESIAN_POINT('Origin',(3.5,2.5,13.8));
#9776=CARTESIAN_POINT('',(4.,0.4,13.8));
#9777=CARTESIAN_POINT('',(4.,1.05,13.8));
#9778=CARTESIAN_POINT('',(3.75,0.4,13.8));
#9779=CARTESIAN_POINT('Origin',(4.,-0.4,13.));
#9780=CARTESIAN_POINT('',(4.,0.4,16.));
#9781=CARTESIAN_POINT('',(4.,0.4,13.));
#9782=CARTESIAN_POINT('',(4.,-0.4,16.));
#9783=CARTESIAN_POINT('',(4.,-0.4,16.));
#9784=CARTESIAN_POINT('',(4.,-0.4,13.));
#9785=CARTESIAN_POINT('',(4.,-0.4,13.));
#9786=CARTESIAN_POINT('',(4.,-0.4,13.));
#9787=CARTESIAN_POINT('Origin',(4.,0.4,13.));
#9788=CARTESIAN_POINT('',(0.916515138991168,0.4,13.));
#9789=CARTESIAN_POINT('',(4.,0.4,13.));
#9790=CARTESIAN_POINT('',(0.453899768671455,0.4,13.));
#9791=CARTESIAN_POINT('',(4.,0.4,13.));
#9792=CARTESIAN_POINT('',(0.453899768671455,0.4,13.1));
#9793=CARTESIAN_POINT('',(0.453899768671455,0.4,11.9));
#9794=CARTESIAN_POINT('',(-0.453899768671455,0.4,13.1));
#9795=CARTESIAN_POINT('',(2.,0.4,13.1));
#9796=CARTESIAN_POINT('',(-0.453899768671455,0.4,13.));
#9797=CARTESIAN_POINT('',(-0.453899768671455,0.4,11.9));
#9798=CARTESIAN_POINT('',(-0.916515138991168,0.4,13.));
#9799=CARTESIAN_POINT('',(4.,0.4,13.));
#9800=CARTESIAN_POINT('',(-4.,0.4,13.));
#9801=CARTESIAN_POINT('',(4.,0.4,13.));
#9802=CARTESIAN_POINT('',(-4.,0.4,16.));
#9803=CARTESIAN_POINT('',(-4.,0.4,13.));
#9804=CARTESIAN_POINT('',(4.,0.4,16.));
#9805=CARTESIAN_POINT('Origin',(0.59,0.,12.5));
#9806=CARTESIAN_POINT('',(0.59,0.133884278389959,12.4035634923901));
#9807=CARTESIAN_POINT('',(0.59,0.133884278389959,12.5964365076099));
#9808=CARTESIAN_POINT('',(0.59,0.133884278389959,11.9));
#9809=CARTESIAN_POINT('Origin',(0.59,0.,12.5));
#9810=CARTESIAN_POINT('Origin',(0.59,0.,12.5));
#9811=CARTESIAN_POINT('',(0.59,-0.133884278389959,12.4035634923901));
#9812=CARTESIAN_POINT('Ctrl Pts',(0.59,-0.133884278389958,12.4035634923901));
#9813=CARTESIAN_POINT('Ctrl Pts',(0.591198403406107,-0.128603165341392,
12.3962316423768));
#9814=CARTESIAN_POINT('Ctrl Pts',(0.59244064128815,-0.122792448979943,12.3894472111884));
#9815=CARTESIAN_POINT('Ctrl Pts',(0.596510641114135,-0.10208383195986,12.3687385941683));
#9816=CARTESIAN_POINT('Ctrl Pts',(0.599544094983168,-0.0836002135946602,
12.3560565239921));
#9817=CARTESIAN_POINT('Ctrl Pts',(0.603817074382983,-0.0429774150042656,
12.3391843843662));
#9818=CARTESIAN_POINT('Ctrl Pts',(0.605,-0.0208299403327841,12.335));
#9819=CARTESIAN_POINT('Ctrl Pts',(0.605,0.020829940332784,12.335));
#9820=CARTESIAN_POINT('Ctrl Pts',(0.603817074382983,0.0429774150042655,
12.3391843843662));
#9821=CARTESIAN_POINT('Ctrl Pts',(0.599544094983168,0.0836002135946602,
12.3560565239921));
#9822=CARTESIAN_POINT('Ctrl Pts',(0.596510641114135,0.10208383195986,12.3687385941683));
#9823=CARTESIAN_POINT('Ctrl Pts',(0.59244064128815,0.122792448979943,12.3894472111884));
#9824=CARTESIAN_POINT('Ctrl Pts',(0.591198403406107,0.128603165341392,12.3962316423768));
#9825=CARTESIAN_POINT('Ctrl Pts',(0.59,0.133884278389958,12.4035634923901));
#9826=CARTESIAN_POINT('',(0.59,-0.133884278389959,12.5964365076099));
#9827=CARTESIAN_POINT('Origin',(0.59,0.,12.5));
#9828=CARTESIAN_POINT('',(0.605,3.67341977584082E-17,12.665));
#9829=CARTESIAN_POINT('Ctrl Pts',(0.605,7.63278329429795E-17,12.665));
#9830=CARTESIAN_POINT('Ctrl Pts',(0.605,-0.020829940332784,12.665));
#9831=CARTESIAN_POINT('Ctrl Pts',(0.603817074382983,-0.0429774150042655,
12.6608156156338));
#9832=CARTESIAN_POINT('Ctrl Pts',(0.599544094983168,-0.0836002135946602,
12.6439434760079));
#9833=CARTESIAN_POINT('Ctrl Pts',(0.596510641114135,-0.10208383195986,12.6312614058317));
#9834=CARTESIAN_POINT('Ctrl Pts',(0.59244064128815,-0.122792448979942,12.6105527888116));
#9835=CARTESIAN_POINT('Ctrl Pts',(0.591198403406107,-0.128603165341392,
12.6037683576232));
#9836=CARTESIAN_POINT('Ctrl Pts',(0.59,-0.133884278389959,12.5964365076099));
#9837=CARTESIAN_POINT('',(1.,-2.02066721859312E-17,12.665));
#9838=CARTESIAN_POINT('',(0.59,-2.02066721859312E-17,12.665));
#9839=CARTESIAN_POINT('',(0.986293566845085,0.164999999999999,12.5));
#9840=CARTESIAN_POINT('Ctrl Pts',(0.986293566845085,0.164999999999999,12.5));
#9841=CARTESIAN_POINT('Ctrl Pts',(0.986293566845085,0.164999999999999,12.4792411222579));
#9842=CARTESIAN_POINT('Ctrl Pts',(0.987016731044511,0.160843546393744,12.4571250491954));
#9843=CARTESIAN_POINT('Ctrl Pts',(0.989615421633511,0.143993021293681,12.4164840215393));
#9844=CARTESIAN_POINT('Ctrl Pts',(0.991451962924594,0.131300979727688,12.3979557419361));
#9845=CARTESIAN_POINT('Ctrl Pts',(0.994888849961666,0.102044633178354,12.3686993953868));
#9846=CARTESIAN_POINT('Ctrl Pts',(0.996714420415386,0.0835161924492572,
12.3560070595837));
#9847=CARTESIAN_POINT('Ctrl Pts',(0.99928792543863,0.0428746115883117,12.3391563208071));
#9848=CARTESIAN_POINT('Ctrl Pts',(1.,0.0207583454229728,12.335));
#9849=CARTESIAN_POINT('Ctrl Pts',(1.,-0.0207583454229728,12.335));
#9850=CARTESIAN_POINT('Ctrl Pts',(0.99928792543863,-0.0428746115883117,
12.3391563208071));
#9851=CARTESIAN_POINT('Ctrl Pts',(0.996714420415386,-0.0835161924492572,
12.3560070595837));
#9852=CARTESIAN_POINT('Ctrl Pts',(0.994888849961666,-0.102044633178354,
12.3686993953868));
#9853=CARTESIAN_POINT('Ctrl Pts',(0.991451962924594,-0.131300979727688,
12.3979557419361));
#9854=CARTESIAN_POINT('Ctrl Pts',(0.989615421633511,-0.143993021293681,
12.4164840215393));
#9855=CARTESIAN_POINT('Ctrl Pts',(0.987016731044511,-0.160843546393744,
12.4571250491954));
#9856=CARTESIAN_POINT('Ctrl Pts',(0.986293566845085,-0.164999999999999,
12.4792411222579));
#9857=CARTESIAN_POINT('Ctrl Pts',(0.986293566845085,-0.164999999999999,
12.5207588777421));
#9858=CARTESIAN_POINT('Ctrl Pts',(0.987016731044511,-0.160843546393744,
12.5428749508046));
#9859=CARTESIAN_POINT('Ctrl Pts',(0.989615421633511,-0.143993021293681,
12.5835159784607));
#9860=CARTESIAN_POINT('Ctrl Pts',(0.991451962924594,-0.131300979727688,
12.6020442580639));
#9861=CARTESIAN_POINT('Ctrl Pts',(0.994888849961666,-0.102044633178354,
12.6313006046132));
#9862=CARTESIAN_POINT('Ctrl Pts',(0.996714420415386,-0.0835161924492572,
12.6439929404163));
#9863=CARTESIAN_POINT('Ctrl Pts',(0.99928792543863,-0.0428746115883117,
12.6608436791929));
#9864=CARTESIAN_POINT('Ctrl Pts',(1.,-0.0207583454229728,12.665));
#9865=CARTESIAN_POINT('Ctrl Pts',(1.,-4.85722573273506E-17,12.665));
#9866=CARTESIAN_POINT('Ctrl Pts',(1.,-9.36750677027476E-17,12.665));
#9867=CARTESIAN_POINT('Ctrl Pts',(1.,0.0207583454229727,12.665));
#9868=CARTESIAN_POINT('Ctrl Pts',(0.99928792543863,0.0428746115883117,12.6608436791929));
#9869=CARTESIAN_POINT('Ctrl Pts',(0.996714420415386,0.0835161924492572,
12.6439929404163));
#9870=CARTESIAN_POINT('Ctrl Pts',(0.994888849961666,0.102044633178354,12.6313006046132));
#9871=CARTESIAN_POINT('Ctrl Pts',(0.991451962924594,0.131300979727688,12.6020442580639));
#9872=CARTESIAN_POINT('Ctrl Pts',(0.989615421633511,0.143993021293681,12.5835159784607));
#9873=CARTESIAN_POINT('Ctrl Pts',(0.987016731044511,0.160843546393744,12.5428749508046));
#9874=CARTESIAN_POINT('Ctrl Pts',(0.986293566845085,0.164999999999999,12.5207588777421));
#9875=CARTESIAN_POINT('Ctrl Pts',(0.986293566845085,0.164999999999999,12.5));
#9876=CARTESIAN_POINT('Ctrl Pts',(0.59,0.133884278389959,12.5964365076099));
#9877=CARTESIAN_POINT('Ctrl Pts',(0.591198403406107,0.128603165341392,12.6037683576232));
#9878=CARTESIAN_POINT('Ctrl Pts',(0.59244064128815,0.122792448979943,12.6105527888116));
#9879=CARTESIAN_POINT('Ctrl Pts',(0.596510641114135,0.10208383195986,12.6312614058317));
#9880=CARTESIAN_POINT('Ctrl Pts',(0.599544094983168,0.0836002135946602,
12.6439434760079));
#9881=CARTESIAN_POINT('Ctrl Pts',(0.603817074382983,0.0429774150042655,
12.6608156156338));
#9882=CARTESIAN_POINT('Ctrl Pts',(0.605,0.020829940332784,12.665));
#9883=CARTESIAN_POINT('Ctrl Pts',(0.605,-2.77555756156289E-17,12.665));
#9884=CARTESIAN_POINT('Origin',(0.59,0.,12.5));
#9885=CARTESIAN_POINT('',(0.59,-0.133884278389959,11.9));
#9886=CARTESIAN_POINT('Origin',(0.,0.,13.1));
#9887=CARTESIAN_POINT('',(0.453899768671455,-0.4,13.1));
#9888=CARTESIAN_POINT('Origin',(0.,0.,13.1));
#9889=CARTESIAN_POINT('',(-0.453899768671455,-0.4,13.1));
#9890=CARTESIAN_POINT('',(-2.,-0.4,13.1));
#9891=CARTESIAN_POINT('',(-0.605,-7.40911313484149E-17,13.1));
#9892=CARTESIAN_POINT('Origin',(0.,0.,13.1));
#9893=CARTESIAN_POINT('Origin',(0.,0.,13.1));
#9894=CARTESIAN_POINT('Origin',(0.,0.,11.9));
#9895=CARTESIAN_POINT('',(-0.605,-7.40911313484149E-17,12.));
#9896=CARTESIAN_POINT('Origin',(0.,0.,12.));
#9897=CARTESIAN_POINT('',(-0.605,-7.40911313484149E-17,11.9));
#9898=CARTESIAN_POINT('',(-0.453899768671455,-0.4,13.));
#9899=CARTESIAN_POINT('',(-0.453899768671455,-0.4,11.9));
#9900=CARTESIAN_POINT('',(0.453899768671455,-0.4,13.));
#9901=CARTESIAN_POINT('Origin',(0.,0.,13.));
#9902=CARTESIAN_POINT('',(0.453899768671455,-0.4,11.9));
#9903=CARTESIAN_POINT('Origin',(0.,0.,13.));
#9904=CARTESIAN_POINT('Origin',(-4.,-0.4,13.));
#9905=CARTESIAN_POINT('',(0.916515138991168,-0.4,13.));
#9906=CARTESIAN_POINT('',(-4.,-0.4,13.));
#9907=CARTESIAN_POINT('',(-4.,-0.4,13.));
#9908=CARTESIAN_POINT('',(-4.,-0.4,16.));
#9909=CARTESIAN_POINT('',(-4.,-0.4,16.));
#9910=CARTESIAN_POINT('',(-4.,-0.4,13.));
#9911=CARTESIAN_POINT('',(-4.,-0.4,13.));
#9912=CARTESIAN_POINT('',(-0.916515138991168,-0.4,13.));
#9913=CARTESIAN_POINT('',(-4.,-0.4,13.));
#9914=CARTESIAN_POINT('',(-4.,-0.4,13.));
#9915=CARTESIAN_POINT('Origin',(0.,0.,13.));
#9916=CARTESIAN_POINT('Origin',(0.,0.,13.));
#9917=CARTESIAN_POINT('Origin',(0.,0.,13.));
#9918=CARTESIAN_POINT('Origin',(0.,0.,13.));
#9919=CARTESIAN_POINT('Origin',(0.,0.,12.));
#9920=CARTESIAN_POINT('',(-1.,-1.22464679914735E-16,13.));
#9921=CARTESIAN_POINT('Origin',(0.,0.,13.));
#9922=CARTESIAN_POINT('Origin',(0.,0.,13.));
#9923=CARTESIAN_POINT('Origin',(0.,0.,13.));
#9924=CARTESIAN_POINT('',(-1.,-1.22464679914735E-16,12.));
#9925=CARTESIAN_POINT('',(-1.,-1.22464679914735E-16,12.));
#9926=CARTESIAN_POINT('Origin',(0.,0.,12.));
#9927=CARTESIAN_POINT('Origin',(0.,0.,12.));
#9928=CARTESIAN_POINT('Origin',(0.,0.,13.));
#9929=CARTESIAN_POINT('',(-4.,0.4,13.));
#9930=CARTESIAN_POINT('Origin',(0.,0.,13.));
#9931=CARTESIAN_POINT('Origin',(-4.,0.4,13.));
#9932=CARTESIAN_POINT('',(-4.,0.4,16.));
#9933=CARTESIAN_POINT('Origin',(0.,0.,16.));
#9934=CARTESIAN_POINT('',(0.,0.,0.));
#9935=CARTESIAN_POINT('Origin',(4.,4.,11.5));
#9936=CARTESIAN_POINT('',(3.835,4.,11.5));
#9937=CARTESIAN_POINT('Origin',(4.,4.,11.5));
#9938=CARTESIAN_POINT('',(3.835,4.,13.));
#9939=CARTESIAN_POINT('',(3.835,4.,11.5));
#9940=CARTESIAN_POINT('Origin',(4.,4.,13.));
#9941=CARTESIAN_POINT('Origin',(4.,4.,11.5));
#9942=CARTESIAN_POINT('Origin',(4.,4.,7.7));
#9943=CARTESIAN_POINT('',(3.835,4.,7.8));
#9944=CARTESIAN_POINT('Origin',(4.,4.,7.8));
#9945=CARTESIAN_POINT('',(3.835,4.,9.));
#9946=CARTESIAN_POINT('',(3.835,4.,7.7));
#9947=CARTESIAN_POINT('Origin',(4.,4.,9.));
#9948=CARTESIAN_POINT('Origin',(4.,4.,9.));
#9949=CARTESIAN_POINT('Origin',(4.,4.,7.8));
#9950=CARTESIAN_POINT('',(3.6,4.,13.));
#9951=CARTESIAN_POINT('Origin',(4.,4.,13.));
#9952=CARTESIAN_POINT('',(3.6,4.,7.8));
#9953=CARTESIAN_POINT('',(3.6,4.,7.8));
#9954=CARTESIAN_POINT('Origin',(4.,4.,7.8));
#9955=CARTESIAN_POINT('Origin',(4.,4.,13.));
#9956=CARTESIAN_POINT('Origin',(4.,4.,7.8));
#9957=CARTESIAN_POINT('',(0.,0.,0.));
#9958=CARTESIAN_POINT('Origin',(4.,4.,7.28));
#9959=CARTESIAN_POINT('',(3.06,4.,7.28));
#9960=CARTESIAN_POINT('Origin',(4.,4.,7.28));
#9961=CARTESIAN_POINT('',(3.06,4.,7.52));
#9962=CARTESIAN_POINT('',(3.06,4.,7.28));
#9963=CARTESIAN_POINT('Origin',(4.,4.,7.52));
#9964=CARTESIAN_POINT('Origin',(4.,4.,7.52));
#9965=CARTESIAN_POINT('',(3.01,4.,7.52));
#9966=CARTESIAN_POINT('Origin',(4.,4.,7.52));
#9967=CARTESIAN_POINT('Origin',(4.,4.,7.28));
#9968=CARTESIAN_POINT('',(3.01,4.,7.28));
#9969=CARTESIAN_POINT('Origin',(4.,4.,7.28));
#9970=CARTESIAN_POINT('Origin',(4.,4.,7.));
#9971=CARTESIAN_POINT('',(3.01,4.,7.));
#9972=CARTESIAN_POINT('',(3.01,4.,7.));
#9973=CARTESIAN_POINT('Origin',(4.,4.,7.));
#9974=CARTESIAN_POINT('Origin',(4.,4.,7.));
#9975=CARTESIAN_POINT('',(3.775,4.,7.8));
#9976=CARTESIAN_POINT('Origin',(4.,4.,7.8));
#9977=CARTESIAN_POINT('',(3.775,4.,7.));
#9978=CARTESIAN_POINT('',(3.775,4.,7.));
#9979=CARTESIAN_POINT('Origin',(4.,4.,7.));
#9980=CARTESIAN_POINT('Origin',(4.,4.,7.));
#9981=CARTESIAN_POINT('',(3.01,4.,7.8));
#9982=CARTESIAN_POINT('Origin',(4.,4.,7.8));
#9983=CARTESIAN_POINT('',(3.01,4.,7.));
#9984=CARTESIAN_POINT('Origin',(4.,4.,7.8));
#9985=CARTESIAN_POINT('Origin',(4.,4.,7.));
#9986=CARTESIAN_POINT('',(0.,0.,0.));
#9987=CARTESIAN_POINT('Origin',(4.,4.,7.3));
#9988=CARTESIAN_POINT('',(3.06,4.,7.5));
#9989=CARTESIAN_POINT('Origin',(4.,4.,7.5));
#9990=CARTESIAN_POINT('',(3.06,4.,7.3));
#9991=CARTESIAN_POINT('',(3.06,4.,7.3));
#9992=CARTESIAN_POINT('Origin',(4.,4.,7.3));
#9993=CARTESIAN_POINT('Origin',(4.,4.,7.3));
#9994=CARTESIAN_POINT('',(3.,4.,7.5));
#9995=CARTESIAN_POINT('Origin',(4.,4.,7.5));
#9996=CARTESIAN_POINT('',(3.,4.,7.3));
#9997=CARTESIAN_POINT('',(3.,4.,7.3));
#9998=CARTESIAN_POINT('Origin',(4.,4.,7.3));
#9999=CARTESIAN_POINT('Origin',(4.,4.,7.5));
#10000=CARTESIAN_POINT('Origin',(4.,4.,7.3));
#10001=CARTESIAN_POINT('',(0.,0.,0.));
#10002=CARTESIAN_POINT('Origin',(10.,0.,0.));
#10003=CARTESIAN_POINT('',(10.,7.34788079488412E-17,0.6));
#10004=CARTESIAN_POINT('Origin',(10.,0.,0.));
#10005=CARTESIAN_POINT('Origin',(0.05,0.,0.));
#10006=CARTESIAN_POINT('',(0.1,7.34788079488412E-17,0.6));
#10007=CARTESIAN_POINT('Origin',(0.1,0.,0.));
#10008=CARTESIAN_POINT('',(0.,-6.12323399573677E-17,0.5));
#10009=CARTESIAN_POINT('',(0.05,-6.73555739531044E-17,0.55));
#10010=CARTESIAN_POINT('Origin',(0.,0.,0.));
#10011=CARTESIAN_POINT('Origin',(0.,0.,0.));
#10012=CARTESIAN_POINT('',(0.,-7.34788079488412E-17,0.6));
#10013=CARTESIAN_POINT('Origin',(0.,0.,0.));
#10014=CARTESIAN_POINT('',(0.,0.,0.));
#10015=CARTESIAN_POINT('Origin',(0.,-0.4,0.));
#10016=CARTESIAN_POINT('',(-0.1954,-0.4,2.39295984553393E-17));
#10017=CARTESIAN_POINT('Origin',(0.,-0.4,0.));
#10018=CARTESIAN_POINT('Origin',(0.0577350269189626,0.,-0.1));
#10019=CARTESIAN_POINT('',(0.0577350269189626,0.,-0.1));
#10020=CARTESIAN_POINT('',(0.115470053837925,0.,0.));
#10021=CARTESIAN_POINT('',(0.0934187836487032,0.,-0.0381939203391614));
#10022=CARTESIAN_POINT('',(0.0577350269189626,-0.2,-0.1));
#10023=CARTESIAN_POINT('',(0.0577350269189626,0.,-0.1));
#10024=CARTESIAN_POINT('',(0.115470053837925,-0.2,0.));
#10025=CARTESIAN_POINT('',(0.115470053837925,-0.2,0.));
#10026=CARTESIAN_POINT('',(0.115470053837925,0.,0.));
#10027=CARTESIAN_POINT('Origin',(-0.0577350269189626,0.,-0.1));
#10028=CARTESIAN_POINT('',(-0.0577350269189626,0.,-0.1));
#10029=CARTESIAN_POINT('',(0.0561324865405187,0.,-0.1));
#10030=CARTESIAN_POINT('',(-0.0577350269189626,-0.2,-0.1));
#10031=CARTESIAN_POINT('',(-0.0577350269189626,0.,-0.1));
#10032=CARTESIAN_POINT('',(0.0577350269189626,-0.2,-0.1));
#10033=CARTESIAN_POINT('Origin',(-0.115470053837925,0.,-1.38777878078145E-17));
#10034=CARTESIAN_POINT('',(-0.115470053837925,0.,-1.41410031829988E-17));
#10035=CARTESIAN_POINT('',(-0.0797862971081845,0.,-0.0618060796608387));
#10036=CARTESIAN_POINT('',(-0.115470053837925,-0.2,-1.38777878078145E-17));
#10037=CARTESIAN_POINT('',(-0.115470053837925,0.,-1.41410031829988E-17));
#10038=CARTESIAN_POINT('',(-0.0577350269189626,-0.2,-0.1));
#10039=CARTESIAN_POINT('Origin',(-0.0577350269189626,0.,0.1));
#10040=CARTESIAN_POINT('',(-0.0577350269189626,0.,0.1));
#10041=CARTESIAN_POINT('',(-0.0509187836487033,0.,0.111806079660839));
#10042=CARTESIAN_POINT('',(-0.0577350269189626,-0.2,0.1));
#10043=CARTESIAN_POINT('',(-0.0577350269189626,0.,0.1));
#10044=CARTESIAN_POINT('',(-0.115470053837925,-0.2,-1.41410031829988E-17));
#10045=CARTESIAN_POINT('Origin',(0.0577350269189626,0.,0.1));
#10046=CARTESIAN_POINT('',(0.0577350269189626,0.,0.1));
#10047=CARTESIAN_POINT('',(0.113867513459481,0.,0.1));
#10048=CARTESIAN_POINT('',(0.0577350269189626,-0.2,0.1));
#10049=CARTESIAN_POINT('',(0.0577350269189626,0.,0.1));
#10050=CARTESIAN_POINT('',(-0.0577350269189626,-0.2,0.1));
#10051=CARTESIAN_POINT('Origin',(0.115470053837925,0.,0.));
#10052=CARTESIAN_POINT('',(0.122286297108185,0.,-0.0118060796608386));
#10053=CARTESIAN_POINT('',(0.0577350269189626,-0.2,0.1));
#10054=CARTESIAN_POINT('Origin',(0.,-0.2,0.));
#10055=CARTESIAN_POINT('Origin',(0.17,0.,0.));
#10056=CARTESIAN_POINT('',(-0.17,-8.67361737988404E-18,-2.0818995585505E-17));
#10057=CARTESIAN_POINT('Origin',(0.,0.,0.));
#10058=CARTESIAN_POINT('Origin',(0.,-0.015,0.));
#10059=CARTESIAN_POINT('',(-0.1954,-0.0254,-2.39295984553393E-17));
#10060=CARTESIAN_POINT('Origin',(0.,-0.0254,0.));
#10061=CARTESIAN_POINT('',(-0.185,-0.015,-2.2655965784226E-17));
#10062=CARTESIAN_POINT('Origin',(0.,-0.2775,0.));
#10063=CARTESIAN_POINT('',(-0.1954,-0.2775,-2.39295984553393E-17));
#10064=CARTESIAN_POINT('',(0.,0.,0.));
#10065=CARTESIAN_POINT('Origin',(0.3,0.4,0.));
#10066=CARTESIAN_POINT('',(-0.3,0.4,-3.67394039744206E-17));
#10067=CARTESIAN_POINT('Origin',(0.,0.4,0.));
#10068=CARTESIAN_POINT('Origin',(0.,0.375,0.));
#10069=CARTESIAN_POINT('',(-0.35,0.35,-4.28626379701573E-17));
#10070=CARTESIAN_POINT('Origin',(0.,0.35,0.));
#10071=CARTESIAN_POINT('',(-0.325,0.375,-3.9801020972289E-17));
#10072=CARTESIAN_POINT('Origin',(0.,0.19,0.));
#10073=CARTESIAN_POINT('',(-0.35,0.03,-4.28626379701574E-17));
#10074=CARTESIAN_POINT('Origin',(0.,0.03,0.));
#10075=CARTESIAN_POINT('',(-0.35,0.19,-4.28626379701574E-17));
#10076=CARTESIAN_POINT('Origin',(0.,0.0149999999999999,0.));
#10077=CARTESIAN_POINT('',(-0.32,-3.29597460435593E-17,-3.91886975727153E-17));
#10078=CARTESIAN_POINT('Origin',(0.,0.,0.));
#10079=CARTESIAN_POINT('',(-0.335,0.0149999999999999,-4.10256677714363E-17));
#10080=CARTESIAN_POINT('Origin',(0.22,0.,0.));
#10081=CARTESIAN_POINT('',(-0.22,-6.93889390390723E-18,-2.69422295812418E-17));
#10082=CARTESIAN_POINT('Origin',(0.,0.,0.));
#10083=CARTESIAN_POINT('Origin',(0.,-0.02,0.));
#10084=CARTESIAN_POINT('',(-0.1954,-0.0492,2.39295984553393E-17));
#10085=CARTESIAN_POINT('Origin',(0.,-0.0492,0.));
#10086=CARTESIAN_POINT('',(-0.21,-0.02,-2.57175827820944E-17));
#10087=CARTESIAN_POINT('Origin',(0.,-0.8,0.));
#10088=CARTESIAN_POINT('',(-0.1954,-1.5646,2.39295984553393E-17));
#10089=CARTESIAN_POINT('Origin',(0.,-1.5646,0.));
#10090=CARTESIAN_POINT('',(-0.1954,-0.8,-2.39295984553393E-17));
#10091=CARTESIAN_POINT('Origin',(0.,-1.58,0.));
#10092=CARTESIAN_POINT('',(-0.16,-1.6,-1.95943487863577E-17));
#10093=CARTESIAN_POINT('Origin',(0.,-1.6,0.));
#10094=CARTESIAN_POINT('',(-0.18,-1.58,-2.20436423846524E-17));
#10095=CARTESIAN_POINT('Origin',(0.,-1.6,0.));
#10096=CARTESIAN_POINT('Origin',(0.0866025403784439,-0.4,-0.15));
#10097=CARTESIAN_POINT('',(0.173205080756888,-0.4,0.));
#10098=CARTESIAN_POINT('',(0.0866025403784439,-0.4,-0.15));
#10099=CARTESIAN_POINT('',(0.173205080756888,-0.4,0.));
#10100=CARTESIAN_POINT('',(0.0866025403784439,-0.64,-0.15));
#10101=CARTESIAN_POINT('',(0.0866025403784439,-0.4,-0.15));
#10102=CARTESIAN_POINT('',(0.173205080756888,-0.64,0.));
#10103=CARTESIAN_POINT('',(0.173205080756888,-0.64,0.));
#10104=CARTESIAN_POINT('',(0.173205080756888,-0.4,0.));
#10105=CARTESIAN_POINT('Origin',(-0.0866025403784438,-0.4,-0.15));
#10106=CARTESIAN_POINT('',(-0.0866025403784438,-0.4,-0.15));
#10107=CARTESIAN_POINT('',(0.0866025403784439,-0.4,-0.15));
#10108=CARTESIAN_POINT('',(-0.0866025403784438,-0.64,-0.15));
#10109=CARTESIAN_POINT('',(-0.0866025403784438,-0.4,-0.15));
#10110=CARTESIAN_POINT('',(0.0866025403784439,-0.64,-0.15));
#10111=CARTESIAN_POINT('Origin',(-0.173205080756888,-0.4,-2.77555756156289E-17));
#10112=CARTESIAN_POINT('',(-0.173205080756888,-0.4,-2.12115047744981E-17));
#10113=CARTESIAN_POINT('',(-0.0866025403784438,-0.4,-0.15));
#10114=CARTESIAN_POINT('',(-0.173205080756888,-0.64,-2.77555756156289E-17));
#10115=CARTESIAN_POINT('',(-0.173205080756888,-0.4,-2.12115047744981E-17));
#10116=CARTESIAN_POINT('',(-0.0866025403784438,-0.64,-0.15));
#10117=CARTESIAN_POINT('Origin',(-0.0866025403784439,-0.4,0.15));
#10118=CARTESIAN_POINT('',(-0.0866025403784439,-0.4,0.15));
#10119=CARTESIAN_POINT('',(-0.173205080756888,-0.4,-2.12115047744981E-17));
#10120=CARTESIAN_POINT('',(-0.0866025403784439,-0.64,0.15));
#10121=CARTESIAN_POINT('',(-0.0866025403784439,-0.4,0.15));
#10122=CARTESIAN_POINT('',(-0.173205080756888,-0.64,-2.12115047744981E-17));
#10123=CARTESIAN_POINT('Origin',(0.0866025403784439,-0.4,0.15));
#10124=CARTESIAN_POINT('',(0.0866025403784439,-0.4,0.15));
#10125=CARTESIAN_POINT('',(-0.0866025403784439,-0.4,0.15));
#10126=CARTESIAN_POINT('',(0.0866025403784439,-0.64,0.15));
#10127=CARTESIAN_POINT('',(0.0866025403784439,-0.4,0.15));
#10128=CARTESIAN_POINT('',(-0.0866025403784439,-0.64,0.15));
#10129=CARTESIAN_POINT('Origin',(0.173205080756888,-0.4,0.));
#10130=CARTESIAN_POINT('',(0.0866025403784439,-0.4,0.15));
#10131=CARTESIAN_POINT('',(0.0866025403784439,-0.64,0.15));
#10132=CARTESIAN_POINT('Origin',(0.,-0.4,-2.77555756156289E-17));
#10133=CARTESIAN_POINT('Origin',(0.,-0.64,-2.77555756156289E-17));
#10134=CARTESIAN_POINT('',(0.,0.,0.));
#10135=CARTESIAN_POINT('',(0.,0.,0.));
#10136=CARTESIAN_POINT('',(0.,0.,0.));
#10137=CARTESIAN_POINT('',(0.,0.,0.));
#10138=CARTESIAN_POINT('',(0.,0.,0.));
#10139=CARTESIAN_POINT('',(0.,0.,0.));
#10140=CARTESIAN_POINT('',(0.,0.,0.));
#10141=CARTESIAN_POINT('',(0.,0.,0.));
#10142=CARTESIAN_POINT('',(0.,0.,0.));
#10143=CARTESIAN_POINT('',(0.,0.,0.));
#10144=CARTESIAN_POINT('',(0.,0.,0.));
#10145=CARTESIAN_POINT('',(0.,0.,0.));
#10146=CARTESIAN_POINT('',(0.,0.,0.));
#10147=CARTESIAN_POINT('',(0.,0.,0.));
#10148=CARTESIAN_POINT('',(0.,0.,0.));
#10149=CARTESIAN_POINT('',(0.,0.,0.));
#10150=CARTESIAN_POINT('',(0.,0.,0.));
#10151=CARTESIAN_POINT('',(0.,0.,0.));
#10152=CARTESIAN_POINT('',(0.,0.,5.));
#10153=CARTESIAN_POINT('',(-1.2,-1.2,-1.));
#10154=CARTESIAN_POINT('',(-1.2,1.2,-1.));
#10155=CARTESIAN_POINT('',(1.2,-1.2,-1.));
#10156=CARTESIAN_POINT('',(1.2,1.2,-1.));
#10157=CARTESIAN_POINT('',(1.13137084989848,1.13137084989848,8.4));
#10158=CARTESIAN_POINT('',(-1.13137084989848,1.13137084989848,8.4));
#10159=CARTESIAN_POINT('',(-1.13137084989848,-1.13137084989848,8.4));
#10160=CARTESIAN_POINT('',(1.13137084989848,-1.13137084989848,8.4));
#10161=CARTESIAN_POINT('',(-4.,-3.,-1.));
#10162=CARTESIAN_POINT('',(4.,6.,1.2));
#10163=CARTESIAN_POINT('',(4.,6.,9.));
#10164=CARTESIAN_POINT('',(5.27279220613579,5.27279220613579,-1.));
#10165=CARTESIAN_POINT('',(5.27279220613579,5.27279220613579,-1.57));
#10166=CARTESIAN_POINT('',(5.27279220613579,5.27279220613579,10.));
#10167=CARTESIAN_POINT('',(5.27279220613579,5.27279220613579,10.1));
#10168=CARTESIAN_POINT('',(2.72720779386421,5.27279220613579,-1.));
#10169=CARTESIAN_POINT('',(2.72720779386421,5.27279220613579,-1.57));
#10170=CARTESIAN_POINT('',(2.72720779386421,5.27279220613579,10.));
#10171=CARTESIAN_POINT('',(2.72720779386421,5.27279220613579,10.1));
#10172=CARTESIAN_POINT('',(2.72720779386421,2.72720779386421,-1.));
#10173=CARTESIAN_POINT('',(2.72720779386421,2.72720779386421,-1.57));
#10174=CARTESIAN_POINT('',(2.72720779386421,2.72720779386421,10.));
#10175=CARTESIAN_POINT('',(2.72720779386421,2.72720779386421,10.1));
#10176=CARTESIAN_POINT('',(5.27279220613578,2.72720779386421,-1.));
#10177=CARTESIAN_POINT('',(5.27279220613578,2.72720779386421,-1.57));
#10178=CARTESIAN_POINT('',(5.27279220613578,2.72720779386421,10.));
#10179=CARTESIAN_POINT('',(5.27279220613578,2.72720779386421,10.1));
#10180=CARTESIAN_POINT('',(0.,0.,0.));
#10181=CARTESIAN_POINT('',(0.,0.,0.));
#10182=CARTESIAN_POINT('',(0.,0.,0.));
#10183=CARTESIAN_POINT('',(0.,0.,0.));
#10184=CARTESIAN_POINT('',(0.,0.,3.));
#10185=CARTESIAN_POINT('',(1.,0.,12.5));
#10186=CARTESIAN_POINT('',(4.,4.,13.4));
#10187=CARTESIAN_POINT('',(4.,4.,7.));
#10188=CARTESIAN_POINT('',(0.,0.,0.));
#10189=CARTESIAN_POINT('',(0.,0.,0.));
#10190=UNCERTAINTY_MEASURE_WITH_UNIT(LENGTH_MEASURE(0.001),#10266,
'DISTANCE_ACCURACY_VALUE',
'Maximum model space distance between geometric entities at asserted c
onnectivities');
#10191=UNCERTAINTY_MEASURE_WITH_UNIT(LENGTH_MEASURE(0.001),#10266,
'DISTANCE_ACCURACY_VALUE',
'Maximum model space distance between geometric entities at asserted c
onnectivities');
#10192=UNCERTAINTY_MEASURE_WITH_UNIT(LENGTH_MEASURE(0.001),#10266,
'DISTANCE_ACCURACY_VALUE',
'Maximum model space distance between geometric entities at asserted c
onnectivities');
#10193=UNCERTAINTY_MEASURE_WITH_UNIT(LENGTH_MEASURE(0.001),#10266,
'DISTANCE_ACCURACY_VALUE',
'Maximum model space distance between geometric entities at asserted c
onnectivities');
#10194=UNCERTAINTY_MEASURE_WITH_UNIT(LENGTH_MEASURE(0.001),#10266,
'DISTANCE_ACCURACY_VALUE',
'Maximum model space distance between geometric entities at asserted c
onnectivities');
#10195=UNCERTAINTY_MEASURE_WITH_UNIT(LENGTH_MEASURE(0.001),#10266,
'DISTANCE_ACCURACY_VALUE',
'Maximum model space distance between geometric entities at asserted c
onnectivities');
#10196=UNCERTAINTY_MEASURE_WITH_UNIT(LENGTH_MEASURE(0.001),#10266,
'DISTANCE_ACCURACY_VALUE',
'Maximum model space distance between geometric entities at asserted c
onnectivities');
#10197=UNCERTAINTY_MEASURE_WITH_UNIT(LENGTH_MEASURE(0.001),#10266,
'DISTANCE_ACCURACY_VALUE',
'Maximum model space distance between geometric entities at asserted c
onnectivities');
#10198=UNCERTAINTY_MEASURE_WITH_UNIT(LENGTH_MEASURE(0.001),#10266,
'DISTANCE_ACCURACY_VALUE',
'Maximum model space distance between geometric entities at asserted c
onnectivities');
#10199=UNCERTAINTY_MEASURE_WITH_UNIT(LENGTH_MEASURE(0.001),#10266,
'DISTANCE_ACCURACY_VALUE',
'Maximum model space distance between geometric entities at asserted c
onnectivities');
#10200=UNCERTAINTY_MEASURE_WITH_UNIT(LENGTH_MEASURE(0.001),#10266,
'DISTANCE_ACCURACY_VALUE',
'Maximum model space distance between geometric entities at asserted c
onnectivities');
#10201=UNCERTAINTY_MEASURE_WITH_UNIT(LENGTH_MEASURE(0.001),#10266,
'DISTANCE_ACCURACY_VALUE',
'Maximum model space distance between geometric entities at asserted c
onnectivities');
#10202=UNCERTAINTY_MEASURE_WITH_UNIT(LENGTH_MEASURE(0.001),#10266,
'DISTANCE_ACCURACY_VALUE',
'Maximum model space distance between geometric entities at asserted c
onnectivities');
#10203=UNCERTAINTY_MEASURE_WITH_UNIT(LENGTH_MEASURE(0.001),#10266,
'DISTANCE_ACCURACY_VALUE',
'Maximum model space distance between geometric entities at asserted c
onnectivities');
#10204=UNCERTAINTY_MEASURE_WITH_UNIT(LENGTH_MEASURE(0.001),#10266,
'DISTANCE_ACCURACY_VALUE',
'Maximum model space distance between geometric entities at asserted c
onnectivities');
#10205=UNCERTAINTY_MEASURE_WITH_UNIT(LENGTH_MEASURE(0.001),#10266,
'DISTANCE_ACCURACY_VALUE',
'Maximum model space distance between geometric entities at asserted c
onnectivities');
#10206=UNCERTAINTY_MEASURE_WITH_UNIT(LENGTH_MEASURE(0.001),#10266,
'DISTANCE_ACCURACY_VALUE',
'Maximum model space distance between geometric entities at asserted c
onnectivities');
#10207=UNCERTAINTY_MEASURE_WITH_UNIT(LENGTH_MEASURE(0.001),#10266,
'DISTANCE_ACCURACY_VALUE',
'Maximum model space distance between geometric entities at asserted c
onnectivities');
#10208=UNCERTAINTY_MEASURE_WITH_UNIT(LENGTH_MEASURE(0.001),#10266,
'DISTANCE_ACCURACY_VALUE',
'Maximum model space distance between geometric entities at asserted c
onnectivities');
#10209=UNCERTAINTY_MEASURE_WITH_UNIT(LENGTH_MEASURE(0.001),#10266,
'DISTANCE_ACCURACY_VALUE',
'Maximum model space distance between geometric entities at asserted c
onnectivities');
#10210=UNCERTAINTY_MEASURE_WITH_UNIT(LENGTH_MEASURE(0.001),#10266,
'DISTANCE_ACCURACY_VALUE',
'Maximum model space distance between geometric entities at asserted c
onnectivities');
#10211=UNCERTAINTY_MEASURE_WITH_UNIT(LENGTH_MEASURE(0.001),#10266,
'DISTANCE_ACCURACY_VALUE',
'Maximum model space distance between geometric entities at asserted c
onnectivities');
#10212=UNCERTAINTY_MEASURE_WITH_UNIT(LENGTH_MEASURE(0.001),#10266,
'DISTANCE_ACCURACY_VALUE',
'Maximum model space distance between geometric entities at asserted c
onnectivities');
#10213=UNCERTAINTY_MEASURE_WITH_UNIT(LENGTH_MEASURE(0.001),#10266,
'DISTANCE_ACCURACY_VALUE',
'Maximum model space distance between geometric entities at asserted c
onnectivities');
#10214=UNCERTAINTY_MEASURE_WITH_UNIT(LENGTH_MEASURE(0.001),#10266,
'DISTANCE_ACCURACY_VALUE',
'Maximum model space distance between geometric entities at asserted c
onnectivities');
#10215=UNCERTAINTY_MEASURE_WITH_UNIT(LENGTH_MEASURE(0.001),#10266,
'DISTANCE_ACCURACY_VALUE',
'Maximum model space distance between geometric entities at asserted c
onnectivities');
#10216=UNCERTAINTY_MEASURE_WITH_UNIT(LENGTH_MEASURE(0.001),#10266,
'DISTANCE_ACCURACY_VALUE',
'Maximum model space distance between geometric entities at asserted c
onnectivities');
#10217=UNCERTAINTY_MEASURE_WITH_UNIT(LENGTH_MEASURE(0.001),#10266,
'DISTANCE_ACCURACY_VALUE',
'Maximum model space distance between geometric entities at asserted c
onnectivities');
#10218=UNCERTAINTY_MEASURE_WITH_UNIT(LENGTH_MEASURE(0.001),#10266,
'DISTANCE_ACCURACY_VALUE',
'Maximum model space distance between geometric entities at asserted c
onnectivities');
#10219=UNCERTAINTY_MEASURE_WITH_UNIT(LENGTH_MEASURE(0.001),#10266,
'DISTANCE_ACCURACY_VALUE',
'Maximum model space distance between geometric entities at asserted c
onnectivities');
#10220=UNCERTAINTY_MEASURE_WITH_UNIT(LENGTH_MEASURE(0.001),#10266,
'DISTANCE_ACCURACY_VALUE',
'Maximum model space distance between geometric entities at asserted c
onnectivities');
#10221=UNCERTAINTY_MEASURE_WITH_UNIT(LENGTH_MEASURE(0.001),#10266,
'DISTANCE_ACCURACY_VALUE',
'Maximum model space distance between geometric entities at asserted c
onnectivities');
#10222=UNCERTAINTY_MEASURE_WITH_UNIT(LENGTH_MEASURE(0.001),#10266,
'DISTANCE_ACCURACY_VALUE',
'Maximum model space distance between geometric entities at asserted c
onnectivities');
#10223=UNCERTAINTY_MEASURE_WITH_UNIT(LENGTH_MEASURE(0.001),#10266,
'DISTANCE_ACCURACY_VALUE',
'Maximum model space distance between geometric entities at asserted c
onnectivities');
#10224=UNCERTAINTY_MEASURE_WITH_UNIT(LENGTH_MEASURE(0.001),#10266,
'DISTANCE_ACCURACY_VALUE',
'Maximum model space distance between geometric entities at asserted c
onnectivities');
#10225=UNCERTAINTY_MEASURE_WITH_UNIT(LENGTH_MEASURE(0.001),#10266,
'DISTANCE_ACCURACY_VALUE',
'Maximum model space distance between geometric entities at asserted c
onnectivities');
#10226=UNCERTAINTY_MEASURE_WITH_UNIT(LENGTH_MEASURE(0.001),#10266,
'DISTANCE_ACCURACY_VALUE',
'Maximum model space distance between geometric entities at asserted c
onnectivities');
#10227=UNCERTAINTY_MEASURE_WITH_UNIT(LENGTH_MEASURE(0.001),#10266,
'DISTANCE_ACCURACY_VALUE',
'Maximum model space distance between geometric entities at asserted c
onnectivities');
#10228=(
GEOMETRIC_REPRESENTATION_CONTEXT(3)
GLOBAL_UNCERTAINTY_ASSIGNED_CONTEXT((#10190))
GLOBAL_UNIT_ASSIGNED_CONTEXT((#10266,#10268,#10269))
REPRESENTATION_CONTEXT('','3D')
);
#10229=(
GEOMETRIC_REPRESENTATION_CONTEXT(3)
GLOBAL_UNCERTAINTY_ASSIGNED_CONTEXT((#10191))
GLOBAL_UNIT_ASSIGNED_CONTEXT((#10266,#10268,#10269))
REPRESENTATION_CONTEXT('','3D')
);
#10230=(
GEOMETRIC_REPRESENTATION_CONTEXT(3)
GLOBAL_UNCERTAINTY_ASSIGNED_CONTEXT((#10192))
GLOBAL_UNIT_ASSIGNED_CONTEXT((#10266,#10268,#10269))
REPRESENTATION_CONTEXT('','3D')
);
#10231=(
GEOMETRIC_REPRESENTATION_CONTEXT(3)
GLOBAL_UNCERTAINTY_ASSIGNED_CONTEXT((#10193))
GLOBAL_UNIT_ASSIGNED_CONTEXT((#10266,#10268,#10269))
REPRESENTATION_CONTEXT('','3D')
);
#10232=(
GEOMETRIC_REPRESENTATION_CONTEXT(3)
GLOBAL_UNCERTAINTY_ASSIGNED_CONTEXT((#10194))
GLOBAL_UNIT_ASSIGNED_CONTEXT((#10266,#10268,#10269))
REPRESENTATION_CONTEXT('','3D')
);
#10233=(
GEOMETRIC_REPRESENTATION_CONTEXT(3)
GLOBAL_UNCERTAINTY_ASSIGNED_CONTEXT((#10195))
GLOBAL_UNIT_ASSIGNED_CONTEXT((#10266,#10268,#10269))
REPRESENTATION_CONTEXT('','3D')
);
#10234=(
GEOMETRIC_REPRESENTATION_CONTEXT(3)
GLOBAL_UNCERTAINTY_ASSIGNED_CONTEXT((#10196))
GLOBAL_UNIT_ASSIGNED_CONTEXT((#10266,#10268,#10269))
REPRESENTATION_CONTEXT('','3D')
);
#10235=(
GEOMETRIC_REPRESENTATION_CONTEXT(3)
GLOBAL_UNCERTAINTY_ASSIGNED_CONTEXT((#10197))
GLOBAL_UNIT_ASSIGNED_CONTEXT((#10266,#10268,#10269))
REPRESENTATION_CONTEXT('','3D')
);
#10236=(
GEOMETRIC_REPRESENTATION_CONTEXT(3)
GLOBAL_UNCERTAINTY_ASSIGNED_CONTEXT((#10198))
GLOBAL_UNIT_ASSIGNED_CONTEXT((#10266,#10268,#10269))
REPRESENTATION_CONTEXT('','3D')
);
#10237=(
GEOMETRIC_REPRESENTATION_CONTEXT(3)
GLOBAL_UNCERTAINTY_ASSIGNED_CONTEXT((#10199))
GLOBAL_UNIT_ASSIGNED_CONTEXT((#10266,#10268,#10269))
REPRESENTATION_CONTEXT('','3D')
);
#10238=(
GEOMETRIC_REPRESENTATION_CONTEXT(3)
GLOBAL_UNCERTAINTY_ASSIGNED_CONTEXT((#10200))
GLOBAL_UNIT_ASSIGNED_CONTEXT((#10266,#10268,#10269))
REPRESENTATION_CONTEXT('','3D')
);
#10239=(
GEOMETRIC_REPRESENTATION_CONTEXT(3)
GLOBAL_UNCERTAINTY_ASSIGNED_CONTEXT((#10201))
GLOBAL_UNIT_ASSIGNED_CONTEXT((#10266,#10268,#10269))
REPRESENTATION_CONTEXT('','3D')
);
#10240=(
GEOMETRIC_REPRESENTATION_CONTEXT(3)
GLOBAL_UNCERTAINTY_ASSIGNED_CONTEXT((#10202))
GLOBAL_UNIT_ASSIGNED_CONTEXT((#10266,#10268,#10269))
REPRESENTATION_CONTEXT('','3D')
);
#10241=(
GEOMETRIC_REPRESENTATION_CONTEXT(3)
GLOBAL_UNCERTAINTY_ASSIGNED_CONTEXT((#10203))
GLOBAL_UNIT_ASSIGNED_CONTEXT((#10266,#10268,#10269))
REPRESENTATION_CONTEXT('','3D')
);
#10242=(
GEOMETRIC_REPRESENTATION_CONTEXT(3)
GLOBAL_UNCERTAINTY_ASSIGNED_CONTEXT((#10204))
GLOBAL_UNIT_ASSIGNED_CONTEXT((#10266,#10268,#10269))
REPRESENTATION_CONTEXT('','3D')
);
#10243=(
GEOMETRIC_REPRESENTATION_CONTEXT(3)
GLOBAL_UNCERTAINTY_ASSIGNED_CONTEXT((#10205))
GLOBAL_UNIT_ASSIGNED_CONTEXT((#10266,#10268,#10269))
REPRESENTATION_CONTEXT('','3D')
);
#10244=(
GEOMETRIC_REPRESENTATION_CONTEXT(3)
GLOBAL_UNCERTAINTY_ASSIGNED_CONTEXT((#10206))
GLOBAL_UNIT_ASSIGNED_CONTEXT((#10266,#10268,#10269))
REPRESENTATION_CONTEXT('','3D')
);
#10245=(
GEOMETRIC_REPRESENTATION_CONTEXT(3)
GLOBAL_UNCERTAINTY_ASSIGNED_CONTEXT((#10207))
GLOBAL_UNIT_ASSIGNED_CONTEXT((#10266,#10268,#10269))
REPRESENTATION_CONTEXT('','3D')
);
#10246=(
GEOMETRIC_REPRESENTATION_CONTEXT(3)
GLOBAL_UNCERTAINTY_ASSIGNED_CONTEXT((#10208))
GLOBAL_UNIT_ASSIGNED_CONTEXT((#10266,#10268,#10269))
REPRESENTATION_CONTEXT('','3D')
);
#10247=(
GEOMETRIC_REPRESENTATION_CONTEXT(3)
GLOBAL_UNCERTAINTY_ASSIGNED_CONTEXT((#10209))
GLOBAL_UNIT_ASSIGNED_CONTEXT((#10266,#10268,#10269))
REPRESENTATION_CONTEXT('','3D')
);
#10248=(
GEOMETRIC_REPRESENTATION_CONTEXT(3)
GLOBAL_UNCERTAINTY_ASSIGNED_CONTEXT((#10210))
GLOBAL_UNIT_ASSIGNED_CONTEXT((#10266,#10268,#10269))
REPRESENTATION_CONTEXT('','3D')
);
#10249=(
GEOMETRIC_REPRESENTATION_CONTEXT(3)
GLOBAL_UNCERTAINTY_ASSIGNED_CONTEXT((#10211))
GLOBAL_UNIT_ASSIGNED_CONTEXT((#10266,#10268,#10269))
REPRESENTATION_CONTEXT('','3D')
);
#10250=(
GEOMETRIC_REPRESENTATION_CONTEXT(3)
GLOBAL_UNCERTAINTY_ASSIGNED_CONTEXT((#10212))
GLOBAL_UNIT_ASSIGNED_CONTEXT((#10266,#10268,#10269))
REPRESENTATION_CONTEXT('','3D')
);
#10251=(
GEOMETRIC_REPRESENTATION_CONTEXT(3)
GLOBAL_UNCERTAINTY_ASSIGNED_CONTEXT((#10213))
GLOBAL_UNIT_ASSIGNED_CONTEXT((#10266,#10268,#10269))
REPRESENTATION_CONTEXT('','3D')
);
#10252=(
GEOMETRIC_REPRESENTATION_CONTEXT(3)
GLOBAL_UNCERTAINTY_ASSIGNED_CONTEXT((#10214))
GLOBAL_UNIT_ASSIGNED_CONTEXT((#10266,#10268,#10269))
REPRESENTATION_CONTEXT('','3D')
);
#10253=(
GEOMETRIC_REPRESENTATION_CONTEXT(3)
GLOBAL_UNCERTAINTY_ASSIGNED_CONTEXT((#10215))
GLOBAL_UNIT_ASSIGNED_CONTEXT((#10266,#10268,#10269))
REPRESENTATION_CONTEXT('','3D')
);
#10254=(
GEOMETRIC_REPRESENTATION_CONTEXT(3)
GLOBAL_UNCERTAINTY_ASSIGNED_CONTEXT((#10216))
GLOBAL_UNIT_ASSIGNED_CONTEXT((#10266,#10268,#10269))
REPRESENTATION_CONTEXT('','3D')
);
#10255=(
GEOMETRIC_REPRESENTATION_CONTEXT(3)
GLOBAL_UNCERTAINTY_ASSIGNED_CONTEXT((#10217))
GLOBAL_UNIT_ASSIGNED_CONTEXT((#10266,#10268,#10269))
REPRESENTATION_CONTEXT('','3D')
);
#10256=(
GEOMETRIC_REPRESENTATION_CONTEXT(3)
GLOBAL_UNCERTAINTY_ASSIGNED_CONTEXT((#10218))
GLOBAL_UNIT_ASSIGNED_CONTEXT((#10266,#10268,#10269))
REPRESENTATION_CONTEXT('','3D')
);
#10257=(
GEOMETRIC_REPRESENTATION_CONTEXT(3)
GLOBAL_UNCERTAINTY_ASSIGNED_CONTEXT((#10219))
GLOBAL_UNIT_ASSIGNED_CONTEXT((#10266,#10268,#10269))
REPRESENTATION_CONTEXT('','3D')
);
#10258=(
GEOMETRIC_REPRESENTATION_CONTEXT(3)
GLOBAL_UNCERTAINTY_ASSIGNED_CONTEXT((#10220))
GLOBAL_UNIT_ASSIGNED_CONTEXT((#10266,#10268,#10269))
REPRESENTATION_CONTEXT('','3D')
);
#10259=(
GEOMETRIC_REPRESENTATION_CONTEXT(3)
GLOBAL_UNCERTAINTY_ASSIGNED_CONTEXT((#10221))
GLOBAL_UNIT_ASSIGNED_CONTEXT((#10266,#10268,#10269))
REPRESENTATION_CONTEXT('','3D')
);
#10260=(
GEOMETRIC_REPRESENTATION_CONTEXT(3)
GLOBAL_UNCERTAINTY_ASSIGNED_CONTEXT((#10222))
GLOBAL_UNIT_ASSIGNED_CONTEXT((#10266,#10268,#10269))
REPRESENTATION_CONTEXT('','3D')
);
#10261=(
GEOMETRIC_REPRESENTATION_CONTEXT(3)
GLOBAL_UNCERTAINTY_ASSIGNED_CONTEXT((#10223))
GLOBAL_UNIT_ASSIGNED_CONTEXT((#10266,#10268,#10269))
REPRESENTATION_CONTEXT('','3D')
);
#10262=(
GEOMETRIC_REPRESENTATION_CONTEXT(3)
GLOBAL_UNCERTAINTY_ASSIGNED_CONTEXT((#10224))
GLOBAL_UNIT_ASSIGNED_CONTEXT((#10266,#10268,#10269))
REPRESENTATION_CONTEXT('','3D')
);
#10263=(
GEOMETRIC_REPRESENTATION_CONTEXT(3)
GLOBAL_UNCERTAINTY_ASSIGNED_CONTEXT((#10225))
GLOBAL_UNIT_ASSIGNED_CONTEXT((#10266,#10268,#10269))
REPRESENTATION_CONTEXT('','3D')
);
#10264=(
GEOMETRIC_REPRESENTATION_CONTEXT(3)
GLOBAL_UNCERTAINTY_ASSIGNED_CONTEXT((#10226))
GLOBAL_UNIT_ASSIGNED_CONTEXT((#10266,#10268,#10269))
REPRESENTATION_CONTEXT('','3D')
);
#10265=(
GEOMETRIC_REPRESENTATION_CONTEXT(3)
GLOBAL_UNCERTAINTY_ASSIGNED_CONTEXT((#10227))
GLOBAL_UNIT_ASSIGNED_CONTEXT((#10266,#10268,#10269))
REPRESENTATION_CONTEXT('','3D')
);
#10266=(
LENGTH_UNIT()
NAMED_UNIT(*)
SI_UNIT(.CENTI.,.METRE.)
);
#10267=(
LENGTH_UNIT()
NAMED_UNIT(*)
SI_UNIT($,.METRE.)
);
#10268=(
NAMED_UNIT(*)
PLANE_ANGLE_UNIT()
SI_UNIT($,.RADIAN.)
);
#10269=(
NAMED_UNIT(*)
SI_UNIT($,.STERADIAN.)
SOLID_ANGLE_UNIT()
);
#10270=SHAPE_DEFINITION_REPRESENTATION(#10307,#10404);
#10271=SHAPE_DEFINITION_REPRESENTATION(#10308,#10405);
#10272=SHAPE_DEFINITION_REPRESENTATION(#10309,#10406);
#10273=SHAPE_DEFINITION_REPRESENTATION(#10310,#10407);
#10274=SHAPE_DEFINITION_REPRESENTATION(#10311,#10408);
#10275=SHAPE_DEFINITION_REPRESENTATION(#10312,#10409);
#10276=SHAPE_DEFINITION_REPRESENTATION(#10313,#10410);
#10277=SHAPE_DEFINITION_REPRESENTATION(#10314,#10411);
#10278=SHAPE_DEFINITION_REPRESENTATION(#10315,#10412);
#10279=SHAPE_DEFINITION_REPRESENTATION(#10316,#10413);
#10280=SHAPE_DEFINITION_REPRESENTATION(#10317,#10414);
#10281=SHAPE_DEFINITION_REPRESENTATION(#10318,#10415);
#10282=SHAPE_DEFINITION_REPRESENTATION(#10319,#10416);
#10283=SHAPE_DEFINITION_REPRESENTATION(#10320,#10417);
#10284=SHAPE_DEFINITION_REPRESENTATION(#10321,#10418);
#10285=SHAPE_DEFINITION_REPRESENTATION(#10322,#10419);
#10286=SHAPE_DEFINITION_REPRESENTATION(#10323,#10420);
#10287=SHAPE_DEFINITION_REPRESENTATION(#10324,#10421);
#10288=SHAPE_DEFINITION_REPRESENTATION(#10325,#10422);
#10289=SHAPE_DEFINITION_REPRESENTATION(#10326,#10423);
#10290=SHAPE_DEFINITION_REPRESENTATION(#10327,#10424);
#10291=SHAPE_DEFINITION_REPRESENTATION(#10328,#10425);
#10292=SHAPE_DEFINITION_REPRESENTATION(#10329,#10426);
#10293=SHAPE_DEFINITION_REPRESENTATION(#10332,#10427);
#10294=SHAPE_DEFINITION_REPRESENTATION(#10333,#10428);
#10295=SHAPE_DEFINITION_REPRESENTATION(#10334,#10429);
#10296=SHAPE_DEFINITION_REPRESENTATION(#10335,#10430);
#10297=SHAPE_DEFINITION_REPRESENTATION(#10338,#10431);
#10298=SHAPE_DEFINITION_REPRESENTATION(#10339,#10432);
#10299=SHAPE_DEFINITION_REPRESENTATION(#10340,#10433);
#10300=SHAPE_DEFINITION_REPRESENTATION(#10341,#10434);
#10301=SHAPE_DEFINITION_REPRESENTATION(#10342,#10435);
#10302=SHAPE_DEFINITION_REPRESENTATION(#10343,#10436);
#10303=SHAPE_DEFINITION_REPRESENTATION(#10344,#10437);
#10304=SHAPE_DEFINITION_REPRESENTATION(#10345,#10438);
#10305=SHAPE_DEFINITION_REPRESENTATION(#10346,#10439);
#10306=SHAPE_DEFINITION_REPRESENTATION(#10347,#10440);
#10307=PRODUCT_DEFINITION_SHAPE('',$,#10442);
#10308=PRODUCT_DEFINITION_SHAPE('',$,#10443);
#10309=PRODUCT_DEFINITION_SHAPE('',$,#10444);
#10310=PRODUCT_DEFINITION_SHAPE('',$,#10445);
#10311=PRODUCT_DEFINITION_SHAPE('',$,#10446);
#10312=PRODUCT_DEFINITION_SHAPE('',$,#10447);
#10313=PRODUCT_DEFINITION_SHAPE('',$,#10448);
#10314=PRODUCT_DEFINITION_SHAPE('',$,#10449);
#10315=PRODUCT_DEFINITION_SHAPE('',$,#10450);
#10316=PRODUCT_DEFINITION_SHAPE('',$,#10451);
#10317=PRODUCT_DEFINITION_SHAPE('',$,#10452);
#10318=PRODUCT_DEFINITION_SHAPE('',$,#10453);
#10319=PRODUCT_DEFINITION_SHAPE('',$,#10454);
#10320=PRODUCT_DEFINITION_SHAPE('',$,#10455);
#10321=PRODUCT_DEFINITION_SHAPE('',$,#10456);
#10322=PRODUCT_DEFINITION_SHAPE('',$,#10457);
#10323=PRODUCT_DEFINITION_SHAPE('',$,#10458);
#10324=PRODUCT_DEFINITION_SHAPE('',$,#10459);
#10325=PRODUCT_DEFINITION_SHAPE('',$,#10460);
#10326=PRODUCT_DEFINITION_SHAPE('',$,#10461);
#10327=PRODUCT_DEFINITION_SHAPE('',$,#10462);
#10328=PRODUCT_DEFINITION_SHAPE('',$,#10463);
#10329=PRODUCT_DEFINITION_SHAPE('',$,#10464);
#10330=PRODUCT_DEFINITION_SHAPE($,$,#220);
#10331=PRODUCT_DEFINITION_SHAPE($,$,#221);
#10332=PRODUCT_DEFINITION_SHAPE('',$,#10465);
#10333=PRODUCT_DEFINITION_SHAPE('',$,#10466);
#10334=PRODUCT_DEFINITION_SHAPE('',$,#10467);
#10335=PRODUCT_DEFINITION_SHAPE('',$,#10468);
#10336=PRODUCT_DEFINITION_SHAPE($,$,#222);
#10337=PRODUCT_DEFINITION_SHAPE($,$,#223);
#10338=PRODUCT_DEFINITION_SHAPE('',$,#10469);
#10339=PRODUCT_DEFINITION_SHAPE('',$,#10470);
#10340=PRODUCT_DEFINITION_SHAPE('',$,#10471);
#10341=PRODUCT_DEFINITION_SHAPE('',$,#10472);
#10342=PRODUCT_DEFINITION_SHAPE('',$,#10473);
#10343=PRODUCT_DEFINITION_SHAPE('',$,#10474);
#10344=PRODUCT_DEFINITION_SHAPE('',$,#10475);
#10345=PRODUCT_DEFINITION_SHAPE('',$,#10476);
#10346=PRODUCT_DEFINITION_SHAPE('',$,#10477);
#10347=PRODUCT_DEFINITION_SHAPE('',$,#10478);
#10348=PRODUCT_DEFINITION_SHAPE($,$,#224);
#10349=PRODUCT_DEFINITION_SHAPE($,$,#225);
#10350=PRODUCT_DEFINITION_SHAPE($,$,#226);
#10351=PRODUCT_DEFINITION_SHAPE($,$,#227);
#10352=PRODUCT_DEFINITION_SHAPE($,$,#228);
#10353=PRODUCT_DEFINITION_SHAPE($,$,#229);
#10354=PRODUCT_DEFINITION_SHAPE($,$,#230);
#10355=PRODUCT_DEFINITION_SHAPE($,$,#231);
#10356=PRODUCT_DEFINITION_SHAPE($,$,#232);
#10357=PRODUCT_DEFINITION_SHAPE($,$,#233);
#10358=PRODUCT_DEFINITION_SHAPE($,$,#234);
#10359=PRODUCT_DEFINITION_SHAPE($,$,#235);
#10360=PRODUCT_DEFINITION_SHAPE($,$,#236);
#10361=PRODUCT_DEFINITION_SHAPE($,$,#237);
#10362=PRODUCT_DEFINITION_SHAPE($,$,#238);
#10363=PRODUCT_DEFINITION_SHAPE($,$,#239);
#10364=PRODUCT_DEFINITION_SHAPE($,$,#240);
#10365=PRODUCT_DEFINITION_SHAPE($,$,#241);
#10366=PRODUCT_DEFINITION_SHAPE($,$,#242);
#10367=PRODUCT_DEFINITION_SHAPE($,$,#243);
#10368=PRODUCT_DEFINITION_SHAPE($,$,#244);
#10369=PRODUCT_DEFINITION_SHAPE($,$,#245);
#10370=PRODUCT_DEFINITION_SHAPE($,$,#246);
#10371=PRODUCT_DEFINITION_SHAPE($,$,#247);
#10372=PRODUCT_DEFINITION_SHAPE($,$,#248);
#10373=PRODUCT_DEFINITION_SHAPE($,$,#249);
#10374=PRODUCT_DEFINITION_SHAPE($,$,#250);
#10375=PRODUCT_DEFINITION_SHAPE($,$,#251);
#10376=PRODUCT_DEFINITION_SHAPE($,$,#252);
#10377=PRODUCT_DEFINITION_SHAPE($,$,#253);
#10378=PRODUCT_DEFINITION_SHAPE($,$,#254);
#10379=PRODUCT_DEFINITION_SHAPE($,$,#255);
#10380=PRODUCT_DEFINITION_SHAPE($,$,#256);
#10381=PRODUCT_DEFINITION_SHAPE($,$,#257);
#10382=PRODUCT_DEFINITION_SHAPE($,$,#258);
#10383=PRODUCT_DEFINITION_SHAPE($,$,#259);
#10384=PRODUCT_DEFINITION_SHAPE($,$,#260);
#10385=PRODUCT_DEFINITION_SHAPE($,$,#261);
#10386=PRODUCT_DEFINITION_SHAPE($,$,#262);
#10387=PRODUCT_DEFINITION_SHAPE($,$,#263);
#10388=PRODUCT_DEFINITION_SHAPE($,$,#264);
#10389=PRODUCT_DEFINITION_SHAPE($,$,#265);
#10390=PRODUCT_DEFINITION_SHAPE($,$,#266);
#10391=PRODUCT_DEFINITION_SHAPE($,$,#267);
#10392=PRODUCT_DEFINITION_SHAPE($,$,#268);
#10393=PRODUCT_DEFINITION_SHAPE($,$,#269);
#10394=PRODUCT_DEFINITION_SHAPE($,$,#270);
#10395=PRODUCT_DEFINITION_SHAPE($,$,#271);
#10396=PRODUCT_DEFINITION_SHAPE($,$,#272);
#10397=PRODUCT_DEFINITION_SHAPE($,$,#273);
#10398=PRODUCT_DEFINITION_SHAPE($,$,#274);
#10399=PRODUCT_DEFINITION_SHAPE($,$,#275);
#10400=PRODUCT_DEFINITION_SHAPE($,$,#276);
#10401=PRODUCT_DEFINITION_SHAPE($,$,#277);
#10402=PRODUCT_DEFINITION_SHAPE($,$,#278);
#10403=PRODUCT_DEFINITION_SHAPE($,$,#279);
#10404=SHAPE_REPRESENTATION('',(#5432,#6087,#6088),#10228);
#10405=SHAPE_REPRESENTATION('',(#5433,#6033,#6034,#6035,#6036,#6037,#6038,
#6039,#6040,#6041,#6042,#6043,#6044,#6045,#6046,#6047,#6048,#6049,#6050,
#6051,#6052,#6053,#6054,#6055,#6056,#6057,#6058,#6059,#6060,#6061,#6062,
#6063,#6064,#6065,#6066,#6067,#6068,#6069,#6070,#6071,#6072,#6073,#6074,
#6075,#6076,#6077,#6078),#10229);
#10406=SHAPE_REPRESENTATION('',(#5434),#10230);
#10407=SHAPE_REPRESENTATION('',(#5468),#10231);
#10408=SHAPE_REPRESENTATION('',(#5475),#10232);
#10409=SHAPE_REPRESENTATION('',(#5482),#10233);
#10410=SHAPE_REPRESENTATION('',(#5528),#10234);
#10411=SHAPE_REPRESENTATION('',(#5569),#10235);
#10412=SHAPE_REPRESENTATION('',(#5578),#10236);
#10413=SHAPE_REPRESENTATION('',(#5583),#10237);
#10414=SHAPE_REPRESENTATION('',(#5597),#10238);
#10415=SHAPE_REPRESENTATION('',(#5638),#10239);
#10416=SHAPE_REPRESENTATION('',(#5647),#10240);
#10417=SHAPE_REPRESENTATION('',(#5700),#10241);
#10418=SHAPE_REPRESENTATION('',(#5709),#10242);
#10419=SHAPE_REPRESENTATION('',(#5718),#10243);
#10420=SHAPE_REPRESENTATION('',(#5727),#10244);
#10421=SHAPE_REPRESENTATION('',(#5733),#10245);
#10422=SHAPE_REPRESENTATION('',(#5739),#10246);
#10423=SHAPE_REPRESENTATION('',(#5745),#10247);
#10424=SHAPE_REPRESENTATION('',(#5751,#5801,#5802),#10248);
#10425=SHAPE_REPRESENTATION('',(#5752),#10249);
#10426=SHAPE_REPRESENTATION('',(#5784),#10250);
#10427=SHAPE_REPRESENTATION('',(#5803),#10251);
#10428=SHAPE_REPRESENTATION('',(#5829,#5871,#5872),#10252);
#10429=SHAPE_REPRESENTATION('',(#5830),#10253);
#10430=SHAPE_REPRESENTATION('',(#5858),#10254);
#10431=SHAPE_REPRESENTATION('',(#5873),#10255);
#10432=SHAPE_REPRESENTATION('',(#5884),#10256);
#10433=SHAPE_REPRESENTATION('',(#5900,#6079,#6080,#6081,#6082,#6083,#6084,
#6085,#6086),#10257);
#10434=SHAPE_REPRESENTATION('',(#5901),#10258);
#10435=SHAPE_REPRESENTATION('',(#5944),#10259);
#10436=SHAPE_REPRESENTATION('',(#5958),#10260);
#10437=SHAPE_REPRESENTATION('',(#5975),#10261);
#10438=SHAPE_REPRESENTATION('',(#5984),#10262);
#10439=SHAPE_REPRESENTATION('',(#5992),#10263);
#10440=SHAPE_REPRESENTATION('',(#6007),#10264);
#10441=PRODUCT_DEFINITION_CONTEXT('part definition',#10554,'design');
#10442=PRODUCT_DEFINITION('PAT-077',
'PAT-077',#10479,#10441);
#10443=PRODUCT_DEFINITION('Mounting body and return spring',
'Mounting body and return spring',#10480,#10441);
#10444=PRODUCT_DEFINITION('Mounting plate','Mounting plate',#10481,#10441);
#10445=PRODUCT_DEFINITION('Foot strip','Foot strip',#10482,#10441);
#10446=PRODUCT_DEFINITION('Foot strip (1)','Foot strip (1)',#10483,#10441);
#10447=PRODUCT_DEFINITION('Guide body','Guide body',#10484,#10441);
#10448=PRODUCT_DEFINITION('Guide cap','Guide cap',#10485,#10441);
#10449=PRODUCT_DEFINITION('Retracted stop sleeve',
'Retracted stop sleeve',#10486,#10441);
#10450=PRODUCT_DEFINITION('Installed return spring',
'Installed return spring',#10487,#10441);
#10451=PRODUCT_DEFINITION('Extended travel stop frame',
'Extended travel stop frame',#10488,#10441);
#10452=PRODUCT_DEFINITION('Cylinder bottom cap','Cylinder bottom cap',#10489,
#10441);
#10453=PRODUCT_DEFINITION('Barrel gasket','Barrel gasket',#10490,#10441);
#10454=PRODUCT_DEFINITION('Cylinder top cap','Cylinder top cap',#10491,
#10441);
#10455=PRODUCT_DEFINITION('Barrel gasket (1)','Barrel gasket (1)',#10492,
#10441);
#10456=PRODUCT_DEFINITION('Cylinder tube','Cylinder tube',#10493,#10441);
#10457=PRODUCT_DEFINITION('Rod seal envelope','Rod seal envelope',#10494,
#10441);
#10458=PRODUCT_DEFINITION('M5 tie rod','M5 tie rod',#10495,#10441);
#10459=PRODUCT_DEFINITION('M5 tie rod (1)','M5 tie rod (1)',#10496,#10441);
#10460=PRODUCT_DEFINITION('M5 tie rod (2)','M5 tie rod (2)',#10497,#10441);
#10461=PRODUCT_DEFINITION('M5 tie rod (3)','M5 tie rod (3)',#10498,#10441);
#10462=PRODUCT_DEFINITION('Linear Ball Bushing - 12 x 21 x 30 mm',
'Linear Ball Bushing - 12 x 21 x 30 mm',#10499,#10441);
#10463=PRODUCT_DEFINITION('Steel sleeve','Steel sleeve',#10500,#10441);
#10464=PRODUCT_DEFINITION('Ball retainer (plastic)',
'Ball retainer (plastic)',#10501,#10441);
#10465=PRODUCT_DEFINITION('Cap Screw - M5x20','Cap Screw - M5x20',#10502,
#10441);
#10466=PRODUCT_DEFINITION(
'Push-In Tube Fitting - 6 mm Tube, 1-8 Inch Tapered Pipe Thread',
'Push-In Tube Fitting - 6 mm Tube, 1-8 Inch Tapered Pipe Thread',#10503,
#10441);
#10467=PRODUCT_DEFINITION('Body','Body',#10504,#10441);
#10468=PRODUCT_DEFINITION('Release collar','Release collar',#10505,#10441);
#10469=PRODUCT_DEFINITION('Flat Washer - M5','Flat Washer - M5',#10506,
#10441);
#10470=PRODUCT_DEFINITION('Hex Nut - M5','Hex Nut - M5',#10507,#10441);
#10471=PRODUCT_DEFINITION('Blade, shaft and piston',
'Blade, shaft and piston',#10508,#10441);
#10472=PRODUCT_DEFINITION('Stop blade','Stop blade',#10509,#10441);
#10473=PRODUCT_DEFINITION('Piston rod','Piston rod',#10510,#10441);
#10474=PRODUCT_DEFINITION('Piston','Piston',#10511,#10441);
#10475=PRODUCT_DEFINITION('Piston seal envelope','Piston seal envelope',
#10512,#10441);
#10476=PRODUCT_DEFINITION('100 mm guide shaft','100 mm guide shaft',#10513,
#10441);
#10477=PRODUCT_DEFINITION('M4x4 shaft screw','M4x4 shaft screw',#10514,
#10441);
#10478=PRODUCT_DEFINITION('Cap Screw - M4x16','Cap Screw - M4x16',#10515,
#10441);
#10479=PRODUCT_DEFINITION_FORMATION('',$,#10556);
#10480=PRODUCT_DEFINITION_FORMATION('',$,#10557);
#10481=PRODUCT_DEFINITION_FORMATION('',$,#10558);
#10482=PRODUCT_DEFINITION_FORMATION('',$,#10559);
#10483=PRODUCT_DEFINITION_FORMATION('',$,#10560);
#10484=PRODUCT_DEFINITION_FORMATION('',$,#10561);
#10485=PRODUCT_DEFINITION_FORMATION('',$,#10562);
#10486=PRODUCT_DEFINITION_FORMATION('',$,#10563);
#10487=PRODUCT_DEFINITION_FORMATION('',$,#10564);
#10488=PRODUCT_DEFINITION_FORMATION('',$,#10565);
#10489=PRODUCT_DEFINITION_FORMATION('',$,#10566);
#10490=PRODUCT_DEFINITION_FORMATION('',$,#10567);
#10491=PRODUCT_DEFINITION_FORMATION('',$,#10568);
#10492=PRODUCT_DEFINITION_FORMATION('',$,#10569);
#10493=PRODUCT_DEFINITION_FORMATION('',$,#10570);
#10494=PRODUCT_DEFINITION_FORMATION('',$,#10571);
#10495=PRODUCT_DEFINITION_FORMATION('',$,#10572);
#10496=PRODUCT_DEFINITION_FORMATION('',$,#10573);
#10497=PRODUCT_DEFINITION_FORMATION('',$,#10574);
#10498=PRODUCT_DEFINITION_FORMATION('',$,#10575);
#10499=PRODUCT_DEFINITION_FORMATION('',$,#10576);
#10500=PRODUCT_DEFINITION_FORMATION('',$,#10577);
#10501=PRODUCT_DEFINITION_FORMATION('',$,#10578);
#10502=PRODUCT_DEFINITION_FORMATION('',$,#10579);
#10503=PRODUCT_DEFINITION_FORMATION('',$,#10580);
#10504=PRODUCT_DEFINITION_FORMATION('',$,#10581);
#10505=PRODUCT_DEFINITION_FORMATION('',$,#10582);
#10506=PRODUCT_DEFINITION_FORMATION('',$,#10583);
#10507=PRODUCT_DEFINITION_FORMATION('',$,#10584);
#10508=PRODUCT_DEFINITION_FORMATION('',$,#10585);
#10509=PRODUCT_DEFINITION_FORMATION('',$,#10586);
#10510=PRODUCT_DEFINITION_FORMATION('',$,#10587);
#10511=PRODUCT_DEFINITION_FORMATION('',$,#10588);
#10512=PRODUCT_DEFINITION_FORMATION('',$,#10589);
#10513=PRODUCT_DEFINITION_FORMATION('',$,#10590);
#10514=PRODUCT_DEFINITION_FORMATION('',$,#10591);
#10515=PRODUCT_DEFINITION_FORMATION('',$,#10592);
#10516=PRODUCT_RELATED_PRODUCT_CATEGORY('PAT-077','PAT-077',(#10556));
#10517=PRODUCT_RELATED_PRODUCT_CATEGORY(
'Mounting body and return spring','Mounting body and return spring',(#10557));
#10518=PRODUCT_RELATED_PRODUCT_CATEGORY('Mounting plate',
'Mounting plate',(#10558));
#10519=PRODUCT_RELATED_PRODUCT_CATEGORY('Foot strip','Foot strip',(#10559));
#10520=PRODUCT_RELATED_PRODUCT_CATEGORY('Foot strip (1)',
'Foot strip (1)',(#10560));
#10521=PRODUCT_RELATED_PRODUCT_CATEGORY('Guide body','Guide body',(#10561));
#10522=PRODUCT_RELATED_PRODUCT_CATEGORY('Guide cap','Guide cap',(#10562));
#10523=PRODUCT_RELATED_PRODUCT_CATEGORY('Retracted stop sleeve',
'Retracted stop sleeve',(#10563));
#10524=PRODUCT_RELATED_PRODUCT_CATEGORY('Installed return spring',
'Installed return spring',(#10564));
#10525=PRODUCT_RELATED_PRODUCT_CATEGORY('Extended travel stop frame',
'Extended travel stop frame',(#10565));
#10526=PRODUCT_RELATED_PRODUCT_CATEGORY('Cylinder bottom cap',
'Cylinder bottom cap',(#10566));
#10527=PRODUCT_RELATED_PRODUCT_CATEGORY('Barrel gasket','Barrel gasket',
(#10567));
#10528=PRODUCT_RELATED_PRODUCT_CATEGORY('Cylinder top cap',
'Cylinder top cap',(#10568));
#10529=PRODUCT_RELATED_PRODUCT_CATEGORY('Barrel gasket (1)',
'Barrel gasket (1)',(#10569));
#10530=PRODUCT_RELATED_PRODUCT_CATEGORY('Cylinder tube','Cylinder tube',
(#10570));
#10531=PRODUCT_RELATED_PRODUCT_CATEGORY('Rod seal envelope',
'Rod seal envelope',(#10571));
#10532=PRODUCT_RELATED_PRODUCT_CATEGORY('M5 tie rod','M5 tie rod',(#10572));
#10533=PRODUCT_RELATED_PRODUCT_CATEGORY('M5 tie rod (1)',
'M5 tie rod (1)',(#10573));
#10534=PRODUCT_RELATED_PRODUCT_CATEGORY('M5 tie rod (2)',
'M5 tie rod (2)',(#10574));
#10535=PRODUCT_RELATED_PRODUCT_CATEGORY('M5 tie rod (3)',
'M5 tie rod (3)',(#10575));
#10536=PRODUCT_RELATED_PRODUCT_CATEGORY(
'Linear Ball Bushing - 12 x 21 x 30 mm',
'Linear Ball Bushing - 12 x 21 x 30 mm',(#10576));
#10537=PRODUCT_RELATED_PRODUCT_CATEGORY('Steel sleeve','Steel sleeve',(#10577));
#10538=PRODUCT_RELATED_PRODUCT_CATEGORY('Ball retainer (plastic)',
'Ball retainer (plastic)',(#10578));
#10539=PRODUCT_RELATED_PRODUCT_CATEGORY('Cap Screw - M5x20',
'Cap Screw - M5x20',(#10579));
#10540=PRODUCT_RELATED_PRODUCT_CATEGORY(
'Push-In Tube Fitting - 6 mm Tube, 1-8 Inch Tapered Pipe Thread',
'Push-In Tube Fitting - 6 mm Tube, 1-8 Inch Tapered Pipe Thread',(#10580));
#10541=PRODUCT_RELATED_PRODUCT_CATEGORY('Body','Body',(#10581));
#10542=PRODUCT_RELATED_PRODUCT_CATEGORY('Release collar',
'Release collar',(#10582));
#10543=PRODUCT_RELATED_PRODUCT_CATEGORY('Flat Washer - M5',
'Flat Washer - M5',(#10583));
#10544=PRODUCT_RELATED_PRODUCT_CATEGORY('Hex Nut - M5','Hex Nut - M5',(#10584));
#10545=PRODUCT_RELATED_PRODUCT_CATEGORY('Blade, shaft and piston',
'Blade, shaft and piston',(#10585));
#10546=PRODUCT_RELATED_PRODUCT_CATEGORY('Stop blade','Stop blade',(#10586));
#10547=PRODUCT_RELATED_PRODUCT_CATEGORY('Piston rod','Piston rod',(#10587));
#10548=PRODUCT_RELATED_PRODUCT_CATEGORY('Piston','Piston',(#10588));
#10549=PRODUCT_RELATED_PRODUCT_CATEGORY('Piston seal envelope',
'Piston seal envelope',(#10589));
#10550=PRODUCT_RELATED_PRODUCT_CATEGORY('100 mm guide shaft',
'100 mm guide shaft',(#10590));
#10551=PRODUCT_RELATED_PRODUCT_CATEGORY('M4x4 shaft screw',
'M4x4 shaft screw',(#10591));
#10552=PRODUCT_RELATED_PRODUCT_CATEGORY('Cap Screw - M4x16',
'Cap Screw - M4x16',(#10592));
#10553=APPLICATION_PROTOCOL_DEFINITION('international standard',
'automotive_design',2009,#10554);
#10554=APPLICATION_CONTEXT(
'Core Data for Automotive Mechanical Design Process');
#10555=PRODUCT_CONTEXT('part definition',#10554,'mechanical');
#10556=PRODUCT('PAT-077','PAT-077',
'PAT-077',(#10555));
#10557=PRODUCT('Mounting body and return spring',
'Mounting body and return spring','Mounting body and return spring',(#10555));
#10558=PRODUCT('Mounting plate','Mounting plate','Mounting plate',(#10555));
#10559=PRODUCT('Foot strip','Foot strip','Foot strip',(#10555));
#10560=PRODUCT('Foot strip (1)','Foot strip (1)','Foot strip (1)',(#10555));
#10561=PRODUCT('Guide body','Guide body','Guide body',(#10555));
#10562=PRODUCT('Guide cap','Guide cap','Guide cap',(#10555));
#10563=PRODUCT('Retracted stop sleeve','Retracted stop sleeve',
'Retracted stop sleeve',(#10555));
#10564=PRODUCT('Installed return spring','Installed return spring',
'Installed return spring',(#10555));
#10565=PRODUCT('Extended travel stop frame',
'Extended travel stop frame','Extended travel stop frame',(#10555));
#10566=PRODUCT('Cylinder bottom cap','Cylinder bottom cap',
'Cylinder bottom cap',(#10555));
#10567=PRODUCT('Barrel gasket','Barrel gasket','Barrel gasket',(#10555));
#10568=PRODUCT('Cylinder top cap','Cylinder top cap','Cylinder top cap',
(#10555));
#10569=PRODUCT('Barrel gasket (1)','Barrel gasket (1)','Barrel gasket (1)',(#10555));
#10570=PRODUCT('Cylinder tube','Cylinder tube','Cylinder tube',(#10555));
#10571=PRODUCT('Rod seal envelope','Rod seal envelope',
'Rod seal envelope',(#10555));
#10572=PRODUCT('M5 tie rod','M5 tie rod','M5 tie rod',(#10555));
#10573=PRODUCT('M5 tie rod (1)','M5 tie rod (1)','M5 tie rod (1)',(#10555));
#10574=PRODUCT('M5 tie rod (2)','M5 tie rod (2)','M5 tie rod (2)',(#10555));
#10575=PRODUCT('M5 tie rod (3)','M5 tie rod (3)','M5 tie rod (3)',(#10555));
#10576=PRODUCT('Linear Ball Bushing - 12 x 21 x 30 mm',
'Linear Ball Bushing - 12 x 21 x 30 mm',
'Linear Ball Bushing - 12 x 21 x 30 mm',(#10555));
#10577=PRODUCT('Steel sleeve','Steel sleeve','Steel sleeve',(#10555));
#10578=PRODUCT('Ball retainer (plastic)','Ball retainer (plastic)',
'Ball retainer (plastic)',(#10555));
#10579=PRODUCT('Cap Screw - M5x20','Cap Screw - M5x20',
'Cap Screw - M5x20',(#10555));
#10580=PRODUCT(
'Push-In Tube Fitting - 6 mm Tube, 1-8 Inch Tapered Pipe Thread',
'Push-In Tube Fitting - 6 mm Tube, 1-8 Inch Tapered Pipe Thread',
'Push-In Tube Fitting - 6 mm Tube, 1-8 Inch Tapered Pipe Thread',(#10555));
#10581=PRODUCT('Body','Body','Body',(#10555));
#10582=PRODUCT('Release collar','Release collar','Release collar',(#10555));
#10583=PRODUCT('Flat Washer - M5','Flat Washer - M5','Flat Washer - M5',
(#10555));
#10584=PRODUCT('Hex Nut - M5','Hex Nut - M5','Hex Nut - M5',(#10555));
#10585=PRODUCT('Blade, shaft and piston','Blade, shaft and piston',
'Blade, shaft and piston',(#10555));
#10586=PRODUCT('Stop blade','Stop blade','Stop blade',(#10555));
#10587=PRODUCT('Piston rod','Piston rod','Piston rod',(#10555));
#10588=PRODUCT('Piston','Piston','Piston',(#10555));
#10589=PRODUCT('Piston seal envelope','Piston seal envelope',
'Piston seal envelope',(#10555));
#10590=PRODUCT('100 mm guide shaft','100 mm guide shaft',
'100 mm guide shaft',(#10555));
#10591=PRODUCT('M4x4 shaft screw','M4x4 shaft screw','M4x4 shaft screw',
(#10555));
#10592=PRODUCT('Cap Screw - M4x16','Cap Screw - M4x16',
'Cap Screw - M4x16',(#10555));
#10593=PRESENTATION_STYLE_ASSIGNMENT((#10598));
#10594=PRESENTATION_STYLE_ASSIGNMENT((#10599));
#10595=PRESENTATION_STYLE_ASSIGNMENT((#10600));
#10596=PRESENTATION_STYLE_ASSIGNMENT((#10601));
#10597=PRESENTATION_STYLE_ASSIGNMENT((#10602));
#10598=SURFACE_STYLE_USAGE(.BOTH.,#10603);
#10599=SURFACE_STYLE_USAGE(.BOTH.,#10604);
#10600=SURFACE_STYLE_USAGE(.BOTH.,#10605);
#10601=SURFACE_STYLE_USAGE(.BOTH.,#10606);
#10602=SURFACE_STYLE_USAGE(.BOTH.,#10607);
#10603=SURFACE_SIDE_STYLE('',(#10608));
#10604=SURFACE_SIDE_STYLE('',(#10609));
#10605=SURFACE_SIDE_STYLE('',(#10610));
#10606=SURFACE_SIDE_STYLE('',(#10611));
#10607=SURFACE_SIDE_STYLE('',(#10612));
#10608=SURFACE_STYLE_FILL_AREA(#10613);
#10609=SURFACE_STYLE_FILL_AREA(#10614);
#10610=SURFACE_STYLE_FILL_AREA(#10615);
#10611=SURFACE_STYLE_FILL_AREA(#10616);
#10612=SURFACE_STYLE_FILL_AREA(#10617);
#10613=FILL_AREA_STYLE('Steel - Satin',(#10618));
#10614=FILL_AREA_STYLE('CAD Library Painted - Engineering blue',(#10619));
#10615=FILL_AREA_STYLE('CAD Library Painted - Deep blue',(#10620));
#10616=FILL_AREA_STYLE('CAD Library Painted - Steel gray',(#10621));
#10617=FILL_AREA_STYLE('CAD Library Painted - Graphite',(#10622));
#10618=FILL_AREA_STYLE_COLOUR('Steel - Satin',#10623);
#10619=FILL_AREA_STYLE_COLOUR('CAD Library Painted - Engineering blue',
#10624);
#10620=FILL_AREA_STYLE_COLOUR('CAD Library Painted - Deep blue',#10625);
#10621=FILL_AREA_STYLE_COLOUR('CAD Library Painted - Steel gray',#10626);
#10622=FILL_AREA_STYLE_COLOUR('CAD Library Painted - Graphite',#10627);
#10623=COLOUR_RGB('Steel - Satin',0.627450980392157,0.627450980392157,0.627450980392157);
#10624=COLOUR_RGB('CAD Library Painted - Engineering blue',0.12156862745098,
0.356862745098039,0.6);
#10625=COLOUR_RGB('CAD Library Painted - Deep blue',0.0784313725490196,
0.203921568627451,0.349019607843137);
#10626=COLOUR_RGB('CAD Library Painted - Steel gray',0.592156862745098,
0.631372549019608,0.67843137254902);
#10627=COLOUR_RGB('CAD Library Painted - Graphite',0.168627450980392,0.192156862745098,
0.231372549019608);
#10628=COLOUR_RGB('Dark Blue',0.08,0.2,0.34);
#10629=FILL_AREA_STYLE_COLOUR('',#10628);
#10630=FILL_AREA_STYLE('',(#10629));
#10631=SURFACE_STYLE_FILL_AREA(#10630);
#10632=SURFACE_SIDE_STYLE('',(#10631));
#10633=SURFACE_STYLE_USAGE(.BOTH.,#10632);
#10634=PRESENTATION_STYLE_ASSIGNMENT((#10633));
#10635=COLOUR_RGB('Light Blue',0.38,0.62,0.78);
#10636=FILL_AREA_STYLE_COLOUR('',#10635);
#10637=FILL_AREA_STYLE('',(#10636));
#10638=SURFACE_STYLE_FILL_AREA(#10637);
#10639=SURFACE_SIDE_STYLE('',(#10638));
#10640=SURFACE_STYLE_USAGE(.BOTH.,#10639);
#10641=PRESENTATION_STYLE_ASSIGNMENT((#10640));
#10642=COLOUR_RGB('Sky Blue',0.24,0.69,0.87);
#10643=FILL_AREA_STYLE_COLOUR('',#10642);
#10644=FILL_AREA_STYLE('',(#10643));
#10645=SURFACE_STYLE_FILL_AREA(#10644);
#10646=SURFACE_SIDE_STYLE('',(#10645));
#10647=SURFACE_STYLE_USAGE(.BOTH.,#10646);
#10648=PRESENTATION_STYLE_ASSIGNMENT((#10647));
#10649=COLOUR_RGB('Grey',0.48,0.52,0.57);
#10650=FILL_AREA_STYLE_COLOUR('',#10649);
#10651=FILL_AREA_STYLE('',(#10650));
#10652=SURFACE_STYLE_FILL_AREA(#10651);
#10653=SURFACE_SIDE_STYLE('',(#10652));
#10654=SURFACE_STYLE_USAGE(.BOTH.,#10653);
#10655=PRESENTATION_STYLE_ASSIGNMENT((#10654));
#10656=COLOUR_RGB('Black',0.12,0.14,0.17);
#10657=FILL_AREA_STYLE_COLOUR('',#10656);
#10658=FILL_AREA_STYLE('',(#10657));
#10659=SURFACE_STYLE_FILL_AREA(#10658);
#10660=SURFACE_SIDE_STYLE('',(#10659));
#10661=SURFACE_STYLE_USAGE(.BOTH.,#10660);
#10662=PRESENTATION_STYLE_ASSIGNMENT((#10661));
#10663=COLOUR_RGB('Off White',0.89,0.88,0.83);
#10664=FILL_AREA_STYLE_COLOUR('',#10663);
#10665=FILL_AREA_STYLE('',(#10664));
#10666=SURFACE_STYLE_FILL_AREA(#10665);
#10667=SURFACE_SIDE_STYLE('',(#10666));
#10668=SURFACE_STYLE_USAGE(.BOTH.,#10667);
#10669=PRESENTATION_STYLE_ASSIGNMENT((#10668));
ENDSEC;
END-ISO-10303-21;
